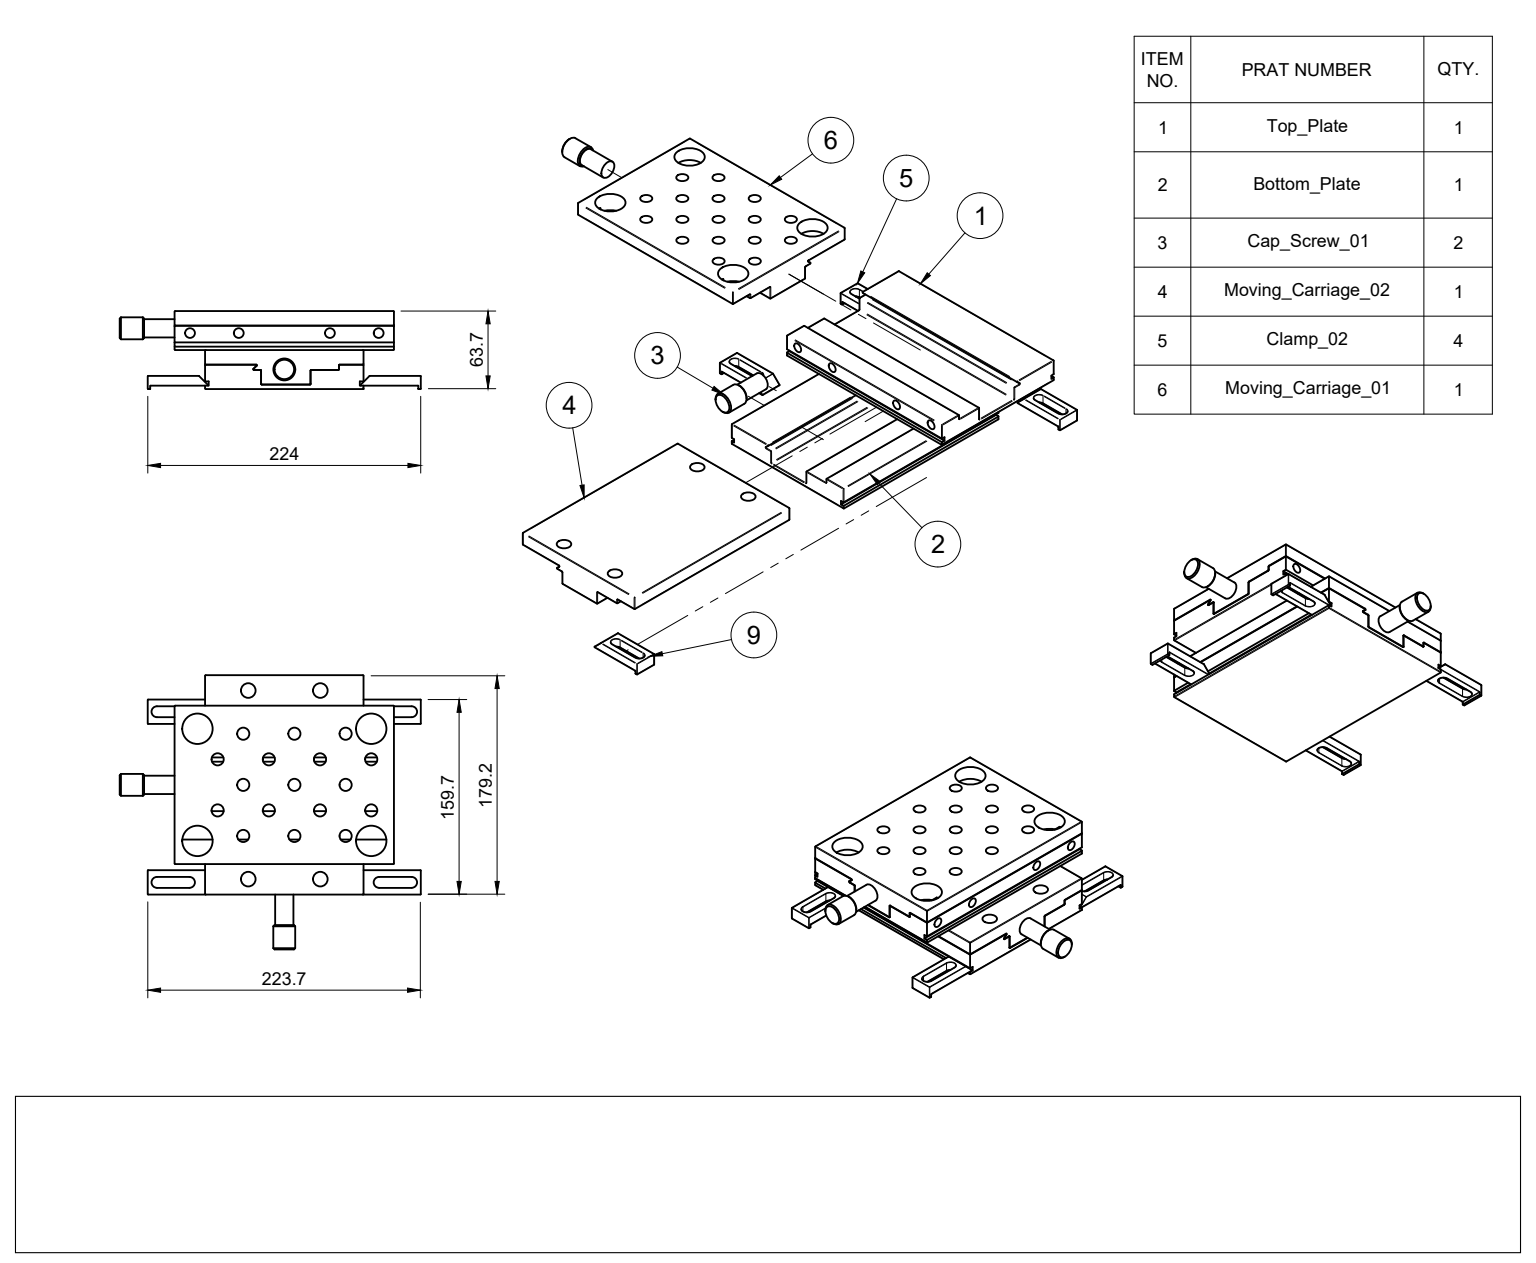
ISO-10303-21;
HEADER;
/* Generated by software containing ST-Developer
 * from STEP Tools, Inc. (www.steptools.com) 
 */

FILE_DESCRIPTION(
/* description */ (''),
/* implementation_level */ '2;1');

FILE_NAME(
/* name */ 'MAS-274',
/* time_stamp */ '2026-10-22T13:39:42+06:00',
/* author */ (''),
/* organization */ (''),
/* preprocessor_version */ 'ST-DEVELOPER v20.2',
/* originating_system */ 'Autodesk Translation Framework v15.15.0.0',
/* authorisation */ '');

FILE_SCHEMA (('AUTOMOTIVE_DESIGN { 1 0 10303 214 3 1 1 }'));
ENDSEC;

DATA;
#10=MECHANICAL_DESIGN_GEOMETRIC_PRESENTATION_REPRESENTATION('',(#307,#308,
#309,#310,#311,#312,#313,#314,#315,#316),#17836);
#11=ITEM_DEFINED_TRANSFORMATION($,$,#9750,#11022);
#12=ITEM_DEFINED_TRANSFORMATION($,$,#9764,#11023);
#13=ITEM_DEFINED_TRANSFORMATION($,$,#9932,#11024);
#14=ITEM_DEFINED_TRANSFORMATION($,$,#10101,#11025);
#15=ITEM_DEFINED_TRANSFORMATION($,$,#10301,#11026);
#16=ITEM_DEFINED_TRANSFORMATION($,$,#10399,#11027);
#17=ITEM_DEFINED_TRANSFORMATION($,$,#10714,#11028);
#18=ITEM_DEFINED_TRANSFORMATION($,$,#10812,#11029);
#19=ITEM_DEFINED_TRANSFORMATION($,$,#10826,#11030);
#20=ITEM_DEFINED_TRANSFORMATION($,$,#10924,#11031);
#21=(
REPRESENTATION_RELATIONSHIP($,$,#17874,#17873)
REPRESENTATION_RELATIONSHIP_WITH_TRANSFORMATION(#11)
SHAPE_REPRESENTATION_RELATIONSHIP()
);
#22=(
REPRESENTATION_RELATIONSHIP($,$,#17875,#17873)
REPRESENTATION_RELATIONSHIP_WITH_TRANSFORMATION(#12)
SHAPE_REPRESENTATION_RELATIONSHIP()
);
#23=(
REPRESENTATION_RELATIONSHIP($,$,#17876,#17873)
REPRESENTATION_RELATIONSHIP_WITH_TRANSFORMATION(#13)
SHAPE_REPRESENTATION_RELATIONSHIP()
);
#24=(
REPRESENTATION_RELATIONSHIP($,$,#17877,#17873)
REPRESENTATION_RELATIONSHIP_WITH_TRANSFORMATION(#14)
SHAPE_REPRESENTATION_RELATIONSHIP()
);
#25=(
REPRESENTATION_RELATIONSHIP($,$,#17878,#17873)
REPRESENTATION_RELATIONSHIP_WITH_TRANSFORMATION(#15)
SHAPE_REPRESENTATION_RELATIONSHIP()
);
#26=(
REPRESENTATION_RELATIONSHIP($,$,#17879,#17873)
REPRESENTATION_RELATIONSHIP_WITH_TRANSFORMATION(#16)
SHAPE_REPRESENTATION_RELATIONSHIP()
);
#27=(
REPRESENTATION_RELATIONSHIP($,$,#17880,#17873)
REPRESENTATION_RELATIONSHIP_WITH_TRANSFORMATION(#17)
SHAPE_REPRESENTATION_RELATIONSHIP()
);
#28=(
REPRESENTATION_RELATIONSHIP($,$,#17881,#17873)
REPRESENTATION_RELATIONSHIP_WITH_TRANSFORMATION(#18)
SHAPE_REPRESENTATION_RELATIONSHIP()
);
#29=(
REPRESENTATION_RELATIONSHIP($,$,#17882,#17873)
REPRESENTATION_RELATIONSHIP_WITH_TRANSFORMATION(#19)
SHAPE_REPRESENTATION_RELATIONSHIP()
);
#30=(
REPRESENTATION_RELATIONSHIP($,$,#17883,#17873)
REPRESENTATION_RELATIONSHIP_WITH_TRANSFORMATION(#20)
SHAPE_REPRESENTATION_RELATIONSHIP()
);
#31=CONTEXT_DEPENDENT_SHAPE_REPRESENTATION(#21,#17863);
#32=CONTEXT_DEPENDENT_SHAPE_REPRESENTATION(#22,#17864);
#33=CONTEXT_DEPENDENT_SHAPE_REPRESENTATION(#23,#17865);
#34=CONTEXT_DEPENDENT_SHAPE_REPRESENTATION(#24,#17866);
#35=CONTEXT_DEPENDENT_SHAPE_REPRESENTATION(#25,#17867);
#36=CONTEXT_DEPENDENT_SHAPE_REPRESENTATION(#26,#17868);
#37=CONTEXT_DEPENDENT_SHAPE_REPRESENTATION(#27,#17869);
#38=CONTEXT_DEPENDENT_SHAPE_REPRESENTATION(#28,#17870);
#39=CONTEXT_DEPENDENT_SHAPE_REPRESENTATION(#29,#17871);
#40=CONTEXT_DEPENDENT_SHAPE_REPRESENTATION(#30,#17872);
#41=NEXT_ASSEMBLY_USAGE_OCCURRENCE('Cap_Screw_01:1','Cap_Screw_01:1',
'Cap_Screw_01:1',#17885,#17886,'Cap_Screw_01:1');
#42=NEXT_ASSEMBLY_USAGE_OCCURRENCE('Bottom_Plate:1','Bottom_Plate:1',
'Bottom_Plate:1',#17885,#17887,'Bottom_Plate:1');
#43=NEXT_ASSEMBLY_USAGE_OCCURRENCE('Moving_Carriage_02:1',
'Moving_Carriage_02:1','Moving_Carriage_02:1',#17885,#17888,
'Moving_Carriage_02:1');
#44=NEXT_ASSEMBLY_USAGE_OCCURRENCE('Top_Plate:1','Top_Plate:1',
'Top_Plate:1',#17885,#17889,'Top_Plate:1');
#45=NEXT_ASSEMBLY_USAGE_OCCURRENCE('Clamp_02:1','Clamp_02:1',
'Clamp_02:1',#17885,#17890,'Clamp_02:1');
#46=NEXT_ASSEMBLY_USAGE_OCCURRENCE('Moving_Carriage_01:1',
'Moving_Carriage_01:1','Moving_Carriage_01:1',#17885,#17891,
'Moving_Carriage_01:1');
#47=NEXT_ASSEMBLY_USAGE_OCCURRENCE('Clamp_01:1','Clamp_01:1',
'Clamp_01:1',#17885,#17892,'Clamp_01:1');
#48=NEXT_ASSEMBLY_USAGE_OCCURRENCE('Cap_Screw_02:1','Cap_Screw_02:1',
'Cap_Screw_02:1',#17885,#17893,'Cap_Screw_02:1');
#49=NEXT_ASSEMBLY_USAGE_OCCURRENCE('Clamp_03:1','Clamp_03:1',
'Clamp_03:1',#17885,#17894,'Clamp_03:1');
#50=NEXT_ASSEMBLY_USAGE_OCCURRENCE('Clamp_04:1','Clamp_04:1',
'Clamp_04:1',#17885,#17895,'Clamp_04:1');
#51=B_SPLINE_CURVE_WITH_KNOTS('',3,(#15627,#15628,#15629,#15630,#15631,
#15632,#15633,#15634,#15635,#15636),.UNSPECIFIED.,.F.,.F.,(4,2,2,2,4),(0.150795783066297,
0.169644465291242,0.188493147516186,0.207360358779659,0.226227570043131),
 .UNSPECIFIED.);
#52=B_SPLINE_CURVE_WITH_KNOTS('',3,(#15640,#15641,#15642,#15643,#15644,
#15645,#15646,#15647,#15648,#15649),.UNSPECIFIED.,.F.,.F.,(4,2,2,2,4),(0.0757694987047649,
0.0947120945274103,0.113654690350056,0.1325089994291,0.151363308508144),
 .UNSPECIFIED.);
#53=B_SPLINE_CURVE_WITH_KNOTS('',3,(#15653,#15654,#15655,#15656,#15657,
#15658,#15659,#15660,#15661,#15662),.UNSPECIFIED.,.F.,.F.,(4,2,2,2,4),(0.151363299946195,
0.170217609025239,0.189071918104283,0.208014513926928,0.226957109749574),
 .UNSPECIFIED.);
#54=B_SPLINE_CURVE_WITH_KNOTS('',3,(#15666,#15667,#15668,#15669,#15670,
#15671,#15672,#15673,#15674,#15675),.UNSPECIFIED.,.F.,.F.,(4,2,2,2,4),(0.0753639993742339,
0.0942312106377064,0.113098421901179,0.131947104126123,0.150795786351068),
 .UNSPECIFIED.);
#55=B_SPLINE_CURVE_WITH_KNOTS('',3,(#15742,#15743,#15744,#15745,#15746,
#15747,#15748,#15749,#15750,#15751),.UNSPECIFIED.,.F.,.F.,(4,2,2,2,4),(0.161501820430177,
0.181202019666624,0.200902218903071,0.22218706551677,0.243471912130469),
 .UNSPECIFIED.);
#56=B_SPLINE_CURVE_WITH_KNOTS('',3,(#15755,#15756,#15757,#15758,#15759,
#15760,#15761,#15762,#15763,#15764),.UNSPECIFIED.,.F.,.F.,(4,2,2,2,4),(0.0930675005857176,
0.116580531967157,0.140093563348597,0.159964165564683,0.179834767780769),
 .UNSPECIFIED.);
#57=B_SPLINE_CURVE_WITH_KNOTS('',3,(#15768,#15769,#15770,#15771,#15772,
#15773,#15774,#15775,#15776,#15777),.UNSPECIFIED.,.F.,.F.,(4,2,2,2,4),(0.179821549944371,
0.199692152160457,0.219562754376543,0.243075785757983,0.266588817139422),
 .UNSPECIFIED.);
#58=B_SPLINE_CURVE_WITH_KNOTS('',3,(#15780,#15781,#15782,#15783,#15784,
#15785,#15786,#15787,#15788,#15789),.UNSPECIFIED.,.F.,.F.,(4,2,2,2,4),(0.0795500677920486,
0.100834914405747,0.122119761019446,0.141819960255893,0.16152015949234),
 .UNSPECIFIED.);
#59=B_SPLINE_CURVE_WITH_KNOTS('',3,(#15810,#15811,#15812,#15813,#15814,
#15815,#15816,#15817,#15818,#15819),.UNSPECIFIED.,.F.,.F.,(4,2,2,2,4),(0.150807296394123,
0.169656833408643,0.188506370423163,0.207379164314979,0.226251958206795),
 .UNSPECIFIED.);
#60=B_SPLINE_CURVE_WITH_KNOTS('',3,(#15822,#15823,#15824,#15825,#15826,
#15827,#15828,#15829,#15830,#15831),.UNSPECIFIED.,.F.,.F.,(4,2,2,2,4),(-0.0760046501525728,
-0.0568078920652052,-0.0376111339778377,-0.0188055669889188,0.),
 .UNSPECIFIED.);
#61=B_SPLINE_CURVE_WITH_KNOTS('',3,(#15833,#15834,#15835,#15836,#15837,
#15838,#15839,#15840,#15841,#15842),.UNSPECIFIED.,.F.,.F.,(4,2,2,2,4),(0.,
0.0188055669889188,0.0376111339778377,0.0568078920652052,0.0760046501525728),
 .UNSPECIFIED.);
#62=B_SPLINE_CURVE_WITH_KNOTS('',3,(#15846,#15847,#15848,#15849,#15850,
#15851,#15852,#15853,#15854,#15855),.UNSPECIFIED.,.F.,.F.,(4,2,2,2,4),(0.0753626345814508,
0.0942354284732671,0.113108222365083,0.131957759379603,0.150807296394123),
 .UNSPECIFIED.);
#63=B_SPLINE_CURVE_WITH_KNOTS('',3,(#15871,#15872,#15873,#15874,#15875,
#15876,#15877,#15878,#15879,#15880),.UNSPECIFIED.,.F.,.F.,(4,2,2,2,4),(0.150807296394123,
0.169656833408643,0.188506370423163,0.207379164314979,0.226251958206795),
 .UNSPECIFIED.);
#64=B_SPLINE_CURVE_WITH_KNOTS('',3,(#15883,#15884,#15885,#15886,#15887,
#15888,#15889,#15890,#15891,#15892),.UNSPECIFIED.,.F.,.F.,(4,2,2,2,4),(-0.0760046501525727,
-0.0568078920652052,-0.0376111339778377,-0.0188055669889188,0.),
 .UNSPECIFIED.);
#65=B_SPLINE_CURVE_WITH_KNOTS('',3,(#15894,#15895,#15896,#15897,#15898,
#15899,#15900,#15901,#15902,#15903),.UNSPECIFIED.,.F.,.F.,(4,2,2,2,4),(0.,
0.0188055669889188,0.0376111339778377,0.0568078920652052,0.0760046501525728),
 .UNSPECIFIED.);
#66=B_SPLINE_CURVE_WITH_KNOTS('',3,(#15907,#15908,#15909,#15910,#15911,
#15912,#15913,#15914,#15915,#15916),.UNSPECIFIED.,.F.,.F.,(4,2,2,2,4),(0.0753626345814508,
0.0942354284732671,0.113108222365083,0.131957759379603,0.150807296394123),
 .UNSPECIFIED.);
#67=B_SPLINE_CURVE_WITH_KNOTS('',3,(#15932,#15933,#15934,#15935,#15936,
#15937,#15938,#15939,#15940,#15941),.UNSPECIFIED.,.F.,.F.,(4,2,2,2,4),(0.150807296394123,
0.169656833408643,0.188506370423163,0.207379164314979,0.226251958206795),
 .UNSPECIFIED.);
#68=B_SPLINE_CURVE_WITH_KNOTS('',3,(#15944,#15945,#15946,#15947,#15948,
#15949,#15950,#15951,#15952,#15953),.UNSPECIFIED.,.F.,.F.,(4,2,2,2,4),(-0.0760046501525728,
-0.0568078920652053,-0.0376111339778377,-0.0188055669889188,0.),
 .UNSPECIFIED.);
#69=B_SPLINE_CURVE_WITH_KNOTS('',3,(#15955,#15956,#15957,#15958,#15959,
#15960,#15961,#15962,#15963,#15964),.UNSPECIFIED.,.F.,.F.,(4,2,2,2,4),(0.,
0.0188055669889189,0.0376111339778377,0.0568078920652053,0.0760046501525728),
 .UNSPECIFIED.);
#70=B_SPLINE_CURVE_WITH_KNOTS('',3,(#15968,#15969,#15970,#15971,#15972,
#15973,#15974,#15975,#15976,#15977),.UNSPECIFIED.,.F.,.F.,(4,2,2,2,4),(0.0753626345814508,
0.0942354284732671,0.113108222365083,0.131957759379603,0.150807296394123),
 .UNSPECIFIED.);
#71=B_SPLINE_CURVE_WITH_KNOTS('',3,(#15990,#15991,#15992,#15993,#15994,
#15995,#15996,#15997,#15998,#15999),.UNSPECIFIED.,.F.,.F.,(4,2,2,2,4),(0.161501820430177,
0.181202019666624,0.200902218903071,0.22218706551677,0.243471912130469),
 .UNSPECIFIED.);
#72=B_SPLINE_CURVE_WITH_KNOTS('',3,(#16003,#16004,#16005,#16006,#16007,
#16008,#16009,#16010,#16011,#16012),.UNSPECIFIED.,.F.,.F.,(4,2,2,2,4),(0.0930675005857173,
0.116580531967157,0.140093563348596,0.159964165564682,0.179834767780769),
 .UNSPECIFIED.);
#73=B_SPLINE_CURVE_WITH_KNOTS('',3,(#16016,#16017,#16018,#16019,#16020,
#16021,#16022,#16023,#16024,#16025),.UNSPECIFIED.,.F.,.F.,(4,2,2,2,4),(0.17982154994437,
0.199692152160456,0.219562754376542,0.243075785757982,0.266588817139421),
 .UNSPECIFIED.);
#74=B_SPLINE_CURVE_WITH_KNOTS('',3,(#16028,#16029,#16030,#16031,#16032,
#16033,#16034,#16035,#16036,#16037),.UNSPECIFIED.,.F.,.F.,(4,2,2,2,4),(0.0795500677920484,
0.100834914405747,0.122119761019446,0.141819960255893,0.16152015949234),
 .UNSPECIFIED.);
#75=B_SPLINE_CURVE_WITH_KNOTS('',3,(#16052,#16053,#16054,#16055,#16056,
#16057,#16058,#16059,#16060,#16061),.UNSPECIFIED.,.F.,.F.,(4,2,2,2,4),(0.150807296394123,
0.169656833408643,0.188506370423163,0.207379164314979,0.226251958206795),
 .UNSPECIFIED.);
#76=B_SPLINE_CURVE_WITH_KNOTS('',3,(#16064,#16065,#16066,#16067,#16068,
#16069,#16070,#16071,#16072,#16073),.UNSPECIFIED.,.F.,.F.,(4,2,2,2,4),(-0.0760046501525727,
-0.0568078920652052,-0.0376111339778377,-0.0188055669889188,0.),
 .UNSPECIFIED.);
#77=B_SPLINE_CURVE_WITH_KNOTS('',3,(#16075,#16076,#16077,#16078,#16079,
#16080,#16081,#16082,#16083,#16084),.UNSPECIFIED.,.F.,.F.,(4,2,2,2,4),(0.,
0.0188055669889188,0.0376111339778377,0.0568078920652052,0.0760046501525727),
 .UNSPECIFIED.);
#78=B_SPLINE_CURVE_WITH_KNOTS('',3,(#16088,#16089,#16090,#16091,#16092,
#16093,#16094,#16095,#16096,#16097),.UNSPECIFIED.,.F.,.F.,(4,2,2,2,4),(0.0753626345814508,
0.0942354284732671,0.113108222365083,0.131957759379603,0.150807296394123),
 .UNSPECIFIED.);
#79=B_SPLINE_CURVE_WITH_KNOTS('',3,(#16107,#16108,#16109,#16110,#16111,
#16112,#16113,#16114,#16115,#16116),.UNSPECIFIED.,.F.,.F.,(4,2,2,2,4),(0.154001562562628,
0.172841700119288,0.191681837675949,0.211603838452167,0.231525839228385),
 .UNSPECIFIED.);
#80=B_SPLINE_CURVE_WITH_KNOTS('',3,(#16120,#16121,#16122,#16123,#16124,
#16125,#16126,#16127,#16128,#16129),.UNSPECIFIED.,.F.,.F.,(4,2,2,2,4),(-0.0796560912226912,
-0.0585074655832388,-0.0373588399437865,-0.0186794199718932,0.),
 .UNSPECIFIED.);
#81=B_SPLINE_CURVE_WITH_KNOTS('',3,(#16133,#16134,#16135,#16136,#16137,
#16138,#16139,#16140,#16141,#16142),.UNSPECIFIED.,.F.,.F.,(4,2,2,2,4),(0.,
0.0186794199718932,0.0373588399437865,0.0585074655832388,0.0796560912226912),
 .UNSPECIFIED.);
#82=B_SPLINE_CURVE_WITH_KNOTS('',3,(#16146,#16147,#16148,#16149,#16150,
#16151,#16152,#16153,#16154,#16155),.UNSPECIFIED.,.F.,.F.,(4,2,2,2,4),(0.0764772858968706,
0.0963992866730888,0.116321287449307,0.135161425005967,0.154001562562628),
 .UNSPECIFIED.);
#83=B_SPLINE_CURVE_WITH_KNOTS('',3,(#16159,#16160,#16161,#16162,#16163,
#16164,#16165,#16166,#16167,#16168,#16169,#16170,#16171,#16172,#16173,#16174,
#16175,#16176,#16177,#16178,#16179),.UNSPECIFIED.,.F.,.F.,(4,2,2,2,3,2,
2,2,2,4),(-0.0487654213288014,-0.0396424658283718,-0.0198212329141859,-0.00991061645709296,
0.,0.00991061645709312,0.0198212329141862,0.0396424658283725,0.0754755088146795,
0.111308551800987),.UNSPECIFIED.);
#84=B_SPLINE_CURVE_WITH_KNOTS('',3,(#16183,#16184,#16185,#16186,#16187,
#16188,#16189,#16190,#16191,#16192,#16193,#16194,#16195,#16196,#16197,#16198),
 .UNSPECIFIED.,.F.,.F.,(4,2,2,2,2,2,2,4),(0.080261889411958,0.100728357288421,
0.121194825164885,0.139914688841483,0.158634552518082,0.177354416194681,
0.19607427987128,0.196799093526934),.UNSPECIFIED.);
#85=B_SPLINE_CURVE_WITH_KNOTS('',3,(#16202,#16203,#16204,#16205,#16206,
#16207,#16208,#16209,#16210,#16211,#16212,#16213,#16214,#16215,#16216,#16217),
 .UNSPECIFIED.,.F.,.F.,(4,2,2,2,2,2,2,4),(0.120470011509229,0.121194825164884,
0.139914688841482,0.158634552518081,0.17735441619468,0.196074279871279,
0.216540747747742,0.237007215624205),.UNSPECIFIED.);
#86=B_SPLINE_CURVE_WITH_KNOTS('',3,(#16221,#16222,#16223,#16224,#16225,
#16226,#16227,#16228,#16229,#16230,#16231,#16232,#16233,#16234,#16235,#16236,
#16237,#16238,#16239,#16240,#16241),.UNSPECIFIED.,.F.,.F.,(4,2,2,2,2,3,
2,2,2,4),(-0.111308551800987,-0.0754755088146795,-0.0396424658283724,-0.0198212329141862,
-0.00991061645709312,0.,0.00991061645709295,0.0198212329141859,0.0396424658283718,
0.0487654212438806),.UNSPECIFIED.);
#87=B_SPLINE_CURVE_WITH_KNOTS('',3,(#16251,#16252,#16253,#16254,#16255,
#16256,#16257,#16258,#16259,#16260),.UNSPECIFIED.,.F.,.F.,(4,2,2,2,4),(0.150795783066297,
0.169644465291242,0.188493147516186,0.207360358779658,0.226227570043131),
 .UNSPECIFIED.);
#88=B_SPLINE_CURVE_WITH_KNOTS('',3,(#16263,#16264,#16265,#16266,#16267,
#16268,#16269,#16270,#16271,#16272),.UNSPECIFIED.,.F.,.F.,(4,2,2,2,4),(0.0757694987047649,
0.0947120945274103,0.113654690350056,0.1325089994291,0.151363308508144),
 .UNSPECIFIED.);
#89=B_SPLINE_CURVE_WITH_KNOTS('',3,(#16274,#16275,#16276,#16277,#16278,
#16279,#16280,#16281,#16282,#16283),.UNSPECIFIED.,.F.,.F.,(4,2,2,2,4),(0.151363299946195,
0.170217609025239,0.189071918104283,0.208014513926928,0.226957109749573),
 .UNSPECIFIED.);
#90=B_SPLINE_CURVE_WITH_KNOTS('',3,(#16287,#16288,#16289,#16290,#16291,
#16292,#16293,#16294,#16295,#16296),.UNSPECIFIED.,.F.,.F.,(4,2,2,2,4),(0.075363999374234,
0.0942312106377065,0.113098421901179,0.131947104126123,0.150795786351068),
 .UNSPECIFIED.);
#91=B_SPLINE_CURVE_WITH_KNOTS('',3,(#16306,#16307,#16308,#16309,#16310,
#16311,#16312,#16313,#16314,#16315),.UNSPECIFIED.,.F.,.F.,(4,2,2,2,4),(0.154001562562628,
0.172841700119289,0.191681837675949,0.211603838452167,0.231525839228385),
 .UNSPECIFIED.);
#92=B_SPLINE_CURVE_WITH_KNOTS('',3,(#16319,#16320,#16321,#16322,#16323,
#16324,#16325,#16326,#16327,#16328),.UNSPECIFIED.,.F.,.F.,(4,2,2,2,4),(-0.0796560912226911,
-0.0585074655832388,-0.0373588399437865,-0.0186794199718933,0.),
 .UNSPECIFIED.);
#93=B_SPLINE_CURVE_WITH_KNOTS('',3,(#16332,#16333,#16334,#16335,#16336,
#16337,#16338,#16339,#16340,#16341),.UNSPECIFIED.,.F.,.F.,(4,2,2,2,4),(0.,
0.0186794199718933,0.0373588399437865,0.0585074655832388,0.0796560912226911),
 .UNSPECIFIED.);
#94=B_SPLINE_CURVE_WITH_KNOTS('',3,(#16345,#16346,#16347,#16348,#16349,
#16350,#16351,#16352,#16353,#16354),.UNSPECIFIED.,.F.,.F.,(4,2,2,2,4),(0.0764772858968706,
0.0963992866730888,0.116321287449307,0.135161425005967,0.154001562562628),
 .UNSPECIFIED.);
#95=B_SPLINE_CURVE_WITH_KNOTS('',3,(#16358,#16359,#16360,#16361,#16362,
#16363,#16364,#16365,#16366,#16367,#16368,#16369,#16370,#16371,#16372,#16373,
#16374,#16375,#16376,#16377,#16378),.UNSPECIFIED.,.F.,.F.,(4,2,2,2,3,2,
2,2,2,4),(-0.0487654213288006,-0.0396424658283715,-0.0198212329141857,-0.00991061645709285,
0.,0.00991061645709304,0.0198212329141861,0.0396424658283721,0.0754755088146788,
0.111308551800986),.UNSPECIFIED.);
#96=B_SPLINE_CURVE_WITH_KNOTS('',3,(#16382,#16383,#16384,#16385,#16386,
#16387,#16388,#16389,#16390,#16391,#16392,#16393,#16394,#16395,#16396,#16397),
 .UNSPECIFIED.,.F.,.F.,(4,2,2,2,2,2,2,4),(0.080261889411958,0.100728357288421,
0.121194825164885,0.139914688841484,0.158634552518082,0.177354416194681,
0.19607427987128,0.196799093526934),.UNSPECIFIED.);
#97=B_SPLINE_CURVE_WITH_KNOTS('',3,(#16401,#16402,#16403,#16404,#16405,
#16406,#16407,#16408,#16409,#16410,#16411,#16412,#16413,#16414,#16415,#16416),
 .UNSPECIFIED.,.F.,.F.,(4,2,2,2,2,2,2,4),(0.120470011509229,0.121194825164884,
0.139914688841482,0.158634552518081,0.17735441619468,0.196074279871279,
0.216540747747742,0.237007215624205),.UNSPECIFIED.);
#98=B_SPLINE_CURVE_WITH_KNOTS('',3,(#16420,#16421,#16422,#16423,#16424,
#16425,#16426,#16427,#16428,#16429,#16430,#16431,#16432,#16433,#16434,#16435,
#16436,#16437,#16438,#16439,#16440),.UNSPECIFIED.,.F.,.F.,(4,2,2,2,2,3,
2,2,2,4),(-0.111308551800986,-0.0754755088146788,-0.0396424658283722,-0.0198212329141861,
-0.00991061645709307,0.,0.00991061645709287,0.0198212329141857,0.0396424658283715,
0.0487654212438799),.UNSPECIFIED.);
#99=B_SPLINE_CURVE_WITH_KNOTS('',3,(#16450,#16451,#16452,#16453,#16454,
#16455,#16456,#16457,#16458,#16459),.UNSPECIFIED.,.F.,.F.,(4,2,2,2,4),(0.154001562562628,
0.172841700119288,0.191681837675949,0.211603838452167,0.231525839228385),
 .UNSPECIFIED.);
#100=B_SPLINE_CURVE_WITH_KNOTS('',3,(#16463,#16464,#16465,#16466,#16467,
#16468,#16469,#16470,#16471,#16472),.UNSPECIFIED.,.F.,.F.,(4,2,2,2,4),(-0.0796560912226909,
-0.0585074655832387,-0.0373588399437865,-0.0186794199718933,0.),
 .UNSPECIFIED.);
#101=B_SPLINE_CURVE_WITH_KNOTS('',3,(#16476,#16477,#16478,#16479,#16480,
#16481,#16482,#16483,#16484,#16485),.UNSPECIFIED.,.F.,.F.,(4,2,2,2,4),(0.,
0.0186794199718933,0.0373588399437866,0.0585074655832387,0.0796560912226909),
 .UNSPECIFIED.);
#102=B_SPLINE_CURVE_WITH_KNOTS('',3,(#16489,#16490,#16491,#16492,#16493,
#16494,#16495,#16496,#16497,#16498),.UNSPECIFIED.,.F.,.F.,(4,2,2,2,4),(0.0764772858968707,
0.0963992866730888,0.116321287449307,0.135161425005967,0.154001562562628),
 .UNSPECIFIED.);
#103=B_SPLINE_CURVE_WITH_KNOTS('',3,(#16502,#16503,#16504,#16505,#16506,
#16507,#16508,#16509,#16510,#16511,#16512,#16513,#16514,#16515,#16516,#16517,
#16518,#16519,#16520,#16521,#16522),.UNSPECIFIED.,.F.,.F.,(4,2,2,2,3,2,
2,2,2,4),(-0.0487654213288013,-0.0396424658283719,-0.019821232914186,-0.00991061645709301,
0.,0.00991061645709316,0.0198212329141863,0.0396424658283726,0.0754755088146797,
0.111308551800987),.UNSPECIFIED.);
#104=B_SPLINE_CURVE_WITH_KNOTS('',3,(#16526,#16527,#16528,#16529,#16530,
#16531,#16532,#16533,#16534,#16535,#16536,#16537,#16538,#16539,#16540,#16541),
 .UNSPECIFIED.,.F.,.F.,(4,2,2,2,2,2,2,4),(0.080261889411958,0.100728357288421,
0.121194825164885,0.139914688841484,0.158634552518082,0.177354416194681,
0.19607427987128,0.196799093526934),.UNSPECIFIED.);
#105=B_SPLINE_CURVE_WITH_KNOTS('',3,(#16545,#16546,#16547,#16548,#16549,
#16550,#16551,#16552,#16553,#16554,#16555,#16556,#16557,#16558,#16559,#16560),
 .UNSPECIFIED.,.F.,.F.,(4,2,2,2,2,2,2,4),(0.120470011509229,0.121194825164884,
0.139914688841482,0.158634552518081,0.17735441619468,0.196074279871279,
0.216540747747742,0.237007215624205),.UNSPECIFIED.);
#106=B_SPLINE_CURVE_WITH_KNOTS('',3,(#16564,#16565,#16566,#16567,#16568,
#16569,#16570,#16571,#16572,#16573,#16574,#16575,#16576,#16577,#16578,#16579,
#16580,#16581,#16582,#16583,#16584),.UNSPECIFIED.,.F.,.F.,(4,2,2,2,2,3,
2,2,2,4),(-0.111308551800987,-0.0754755088146797,-0.0396424658283726,-0.0198212329141863,
-0.00991061645709312,0.,0.00991061645709299,0.019821232914186,0.039642465828372,
0.0487654212438805),.UNSPECIFIED.);
#107=B_SPLINE_CURVE_WITH_KNOTS('',3,(#16594,#16595,#16596,#16597,#16598,
#16599,#16600,#16601,#16602,#16603),.UNSPECIFIED.,.F.,.F.,(4,2,2,2,4),(0.154001562562628,
0.172841700119288,0.191681837675949,0.211603838452167,0.231525839228385),
 .UNSPECIFIED.);
#108=B_SPLINE_CURVE_WITH_KNOTS('',3,(#16607,#16608,#16609,#16610,#16611,
#16612,#16613,#16614,#16615,#16616),.UNSPECIFIED.,.F.,.F.,(4,2,2,2,4),(-0.0796560912226908,
-0.0585074655832387,-0.0373588399437865,-0.0186794199718933,0.),
 .UNSPECIFIED.);
#109=B_SPLINE_CURVE_WITH_KNOTS('',3,(#16620,#16621,#16622,#16623,#16624,
#16625,#16626,#16627,#16628,#16629),.UNSPECIFIED.,.F.,.F.,(4,2,2,2,4),(0.,
0.0186794199718932,0.0373588399437865,0.0585074655832387,0.0796560912226908),
 .UNSPECIFIED.);
#110=B_SPLINE_CURVE_WITH_KNOTS('',3,(#16633,#16634,#16635,#16636,#16637,
#16638,#16639,#16640,#16641,#16642),.UNSPECIFIED.,.F.,.F.,(4,2,2,2,4),(0.0764772858968705,
0.0963992866730887,0.116321287449307,0.135161425005967,0.154001562562628),
 .UNSPECIFIED.);
#111=B_SPLINE_CURVE_WITH_KNOTS('',3,(#16646,#16647,#16648,#16649,#16650,
#16651,#16652,#16653,#16654,#16655,#16656,#16657,#16658,#16659,#16660,#16661,
#16662,#16663,#16664,#16665,#16666),.UNSPECIFIED.,.F.,.F.,(4,2,2,2,3,2,
2,2,2,4),(-0.0487654213288016,-0.0396424658283713,-0.0198212329141857,-0.00991061645709285,
0.,0.0099106164570932,0.0198212329141864,0.0396424658283728,0.0754755088146802,
0.111308551800988),.UNSPECIFIED.);
#112=B_SPLINE_CURVE_WITH_KNOTS('',3,(#16670,#16671,#16672,#16673,#16674,
#16675,#16676,#16677,#16678,#16679,#16680,#16681,#16682,#16683,#16684,#16685),
 .UNSPECIFIED.,.F.,.F.,(4,2,2,2,2,2,2,4),(0.0802618894119582,0.100728357288421,
0.121194825164885,0.139914688841483,0.158634552518082,0.177354416194681,
0.19607427987128,0.196799093526934),.UNSPECIFIED.);
#113=B_SPLINE_CURVE_WITH_KNOTS('',3,(#16689,#16690,#16691,#16692,#16693,
#16694,#16695,#16696,#16697,#16698,#16699,#16700,#16701,#16702,#16703,#16704),
 .UNSPECIFIED.,.F.,.F.,(4,2,2,2,2,2,2,4),(0.12047001150923,0.121194825164884,
0.139914688841483,0.158634552518082,0.17735441619468,0.196074279871279,
0.216540747747742,0.237007215624206),.UNSPECIFIED.);
#114=B_SPLINE_CURVE_WITH_KNOTS('',3,(#16708,#16709,#16710,#16711,#16712,
#16713,#16714,#16715,#16716,#16717,#16718,#16719,#16720,#16721,#16722,#16723,
#16724,#16725,#16726,#16727,#16728),.UNSPECIFIED.,.F.,.F.,(4,2,2,2,2,3,
2,2,2,4),(-0.111308551800987,-0.0754755088146801,-0.0396424658283728,-0.0198212329141864,
-0.00991061645709318,0.,0.00991061645709283,0.0198212329141857,0.0396424658283713,
0.0487654212438809),.UNSPECIFIED.);
#115=B_SPLINE_CURVE_WITH_KNOTS('',3,(#16741,#16742,#16743,#16744,#16745,
#16746,#16747,#16748,#16749,#16750),.UNSPECIFIED.,.F.,.F.,(4,2,2,2,4),(0.161501820430177,
0.181202019666624,0.200902218903071,0.22218706551677,0.243471912130469),
 .UNSPECIFIED.);
#116=B_SPLINE_CURVE_WITH_KNOTS('',3,(#16754,#16755,#16756,#16757,#16758,
#16759,#16760,#16761,#16762,#16763),.UNSPECIFIED.,.F.,.F.,(4,2,2,2,4),(0.0930675005857169,
0.116580531967156,0.140093563348596,0.159964165564682,0.179834767780768),
 .UNSPECIFIED.);
#117=B_SPLINE_CURVE_WITH_KNOTS('',3,(#16767,#16768,#16769,#16770,#16771,
#16772,#16773,#16774,#16775,#16776),.UNSPECIFIED.,.F.,.F.,(4,2,2,2,4),(0.17982154994437,
0.199692152160456,0.219562754376542,0.243075785757982,0.266588817139421),
 .UNSPECIFIED.);
#118=B_SPLINE_CURVE_WITH_KNOTS('',3,(#16779,#16780,#16781,#16782,#16783,
#16784,#16785,#16786,#16787,#16788),.UNSPECIFIED.,.F.,.F.,(4,2,2,2,4),(0.0795500677920484,
0.100834914405747,0.122119761019446,0.141819960255893,0.16152015949234),
 .UNSPECIFIED.);
#119=SPHERICAL_SURFACE('',#9812,0.499999999999998);
#120=SPHERICAL_SURFACE('',#9816,0.499999999999998);
#121=SPHERICAL_SURFACE('',#9821,0.5);
#122=SPHERICAL_SURFACE('',#9827,0.499999999999998);
#123=SPHERICAL_SURFACE('',#9837,0.500000000000007);
#124=SPHERICAL_SURFACE('',#9846,0.500000000000007);
#125=SPHERICAL_SURFACE('',#9859,0.5);
#126=SPHERICAL_SURFACE('',#9863,0.5);
#127=SPHERICAL_SURFACE('',#9868,0.5);
#128=SPHERICAL_SURFACE('',#9874,0.5);
#129=SPHERICAL_SURFACE('',#9883,0.500000000000007);
#130=SPHERICAL_SURFACE('',#9891,0.500000000000007);
#131=SPHERICAL_SURFACE('',#9896,0.500000000000007);
#132=SPHERICAL_SURFACE('',#9902,0.499999999999998);
#133=SPHERICAL_SURFACE('',#9947,0.500000000000025);
#134=SPHERICAL_SURFACE('',#9951,0.500000000000005);
#135=SPHERICAL_SURFACE('',#9977,0.500000000000007);
#136=SPHERICAL_SURFACE('',#9982,0.499999999999998);
#137=SPHERICAL_SURFACE('',#9987,0.500000000000007);
#138=SPHERICAL_SURFACE('',#9991,0.500000000000007);
#139=SPHERICAL_SURFACE('',#9996,0.500000000000007);
#140=SPHERICAL_SURFACE('',#10001,0.500000000000007);
#141=SPHERICAL_SURFACE('',#10006,0.500000000000007);
#142=SPHERICAL_SURFACE('',#10010,0.500000000000007);
#143=SPHERICAL_SURFACE('',#10021,0.500000000000007);
#144=SPHERICAL_SURFACE('',#10030,0.500000000000007);
#145=SPHERICAL_SURFACE('',#10034,0.500000000000007);
#146=SPHERICAL_SURFACE('',#10039,0.499999999999998);
#147=SPHERICAL_SURFACE('',#10043,0.500000000000007);
#148=SPHERICAL_SURFACE('',#10047,0.499999999999998);
#149=SPHERICAL_SURFACE('',#10181,0.499999999999998);
#150=SPHERICAL_SURFACE('',#10185,0.499999999999998);
#151=SPHERICAL_SURFACE('',#10190,0.5);
#152=SPHERICAL_SURFACE('',#10196,0.499999999999998);
#153=SPHERICAL_SURFACE('',#10206,0.500000000000007);
#154=SPHERICAL_SURFACE('',#10215,0.500000000000007);
#155=SPHERICAL_SURFACE('',#10228,0.5);
#156=SPHERICAL_SURFACE('',#10232,0.5);
#157=SPHERICAL_SURFACE('',#10237,0.5);
#158=SPHERICAL_SURFACE('',#10243,0.5);
#159=SPHERICAL_SURFACE('',#10252,0.500000000000007);
#160=SPHERICAL_SURFACE('',#10260,0.500000000000007);
#161=SPHERICAL_SURFACE('',#10265,0.500000000000007);
#162=SPHERICAL_SURFACE('',#10271,0.499999999999998);
#163=SPHERICAL_SURFACE('',#10323,0.299999999999994);
#164=SPHERICAL_SURFACE('',#10334,0.3);
#165=SPHERICAL_SURFACE('',#10338,0.299999999999994);
#166=SPHERICAL_SURFACE('',#10343,0.3);
#167=SPHERICAL_SURFACE('',#10347,0.300000000000011);
#168=SPHERICAL_SURFACE('',#10351,0.300000000000003);
#169=SPHERICAL_SURFACE('',#10355,0.299999999999994);
#170=SPHERICAL_SURFACE('',#10360,0.300000000000011);
#171=SPHERICAL_SURFACE('',#10585,0.500000000000025);
#172=SPHERICAL_SURFACE('',#10588,0.500000000000005);
#173=SPHERICAL_SURFACE('',#10609,0.500000000000007);
#174=SPHERICAL_SURFACE('',#10613,0.499999999999998);
#175=SPHERICAL_SURFACE('',#10618,0.500000000000007);
#176=SPHERICAL_SURFACE('',#10621,0.500000000000007);
#177=SPHERICAL_SURFACE('',#10626,0.500000000000007);
#178=SPHERICAL_SURFACE('',#10630,0.500000000000007);
#179=SPHERICAL_SURFACE('',#10635,0.500000000000007);
#180=SPHERICAL_SURFACE('',#10638,0.500000000000007);
#181=SPHERICAL_SURFACE('',#10648,0.500000000000007);
#182=SPHERICAL_SURFACE('',#10656,0.500000000000007);
#183=SPHERICAL_SURFACE('',#10660,0.500000000000007);
#184=SPHERICAL_SURFACE('',#10664,0.499999999999998);
#185=SPHERICAL_SURFACE('',#10668,0.500000000000007);
#186=SPHERICAL_SURFACE('',#10671,0.499999999999998);
#187=SPHERICAL_SURFACE('',#10736,0.299999999999994);
#188=SPHERICAL_SURFACE('',#10747,0.3);
#189=SPHERICAL_SURFACE('',#10751,0.299999999999994);
#190=SPHERICAL_SURFACE('',#10756,0.3);
#191=SPHERICAL_SURFACE('',#10760,0.300000000000011);
#192=SPHERICAL_SURFACE('',#10764,0.300000000000003);
#193=SPHERICAL_SURFACE('',#10768,0.299999999999994);
#194=SPHERICAL_SURFACE('',#10773,0.300000000000011);
#195=SPHERICAL_SURFACE('',#10848,0.299999999999994);
#196=SPHERICAL_SURFACE('',#10859,0.3);
#197=SPHERICAL_SURFACE('',#10863,0.299999999999994);
#198=SPHERICAL_SURFACE('',#10868,0.3);
#199=SPHERICAL_SURFACE('',#10872,0.300000000000011);
#200=SPHERICAL_SURFACE('',#10876,0.300000000000003);
#201=SPHERICAL_SURFACE('',#10880,0.299999999999994);
#202=SPHERICAL_SURFACE('',#10885,0.300000000000011);
#203=SPHERICAL_SURFACE('',#10946,0.299999999999994);
#204=SPHERICAL_SURFACE('',#10957,0.3);
#205=SPHERICAL_SURFACE('',#10961,0.299999999999994);
#206=SPHERICAL_SURFACE('',#10966,0.3);
#207=SPHERICAL_SURFACE('',#10970,0.300000000000011);
#208=SPHERICAL_SURFACE('',#10974,0.300000000000003);
#209=SPHERICAL_SURFACE('',#10978,0.299999999999994);
#210=SPHERICAL_SURFACE('',#10983,0.300000000000011);
#211=TOROIDAL_SURFACE('',#9804,0.999999999999996,0.500000000000007);
#212=TOROIDAL_SURFACE('',#9808,1.,0.500000000000007);
#213=TOROIDAL_SURFACE('',#9833,0.999999999999996,0.500000000000007);
#214=TOROIDAL_SURFACE('',#9840,1.,0.500000000000007);
#215=TOROIDAL_SURFACE('',#9849,1.,0.500000000000007);
#216=TOROIDAL_SURFACE('',#9853,1.,0.500000000000007);
#217=TOROIDAL_SURFACE('',#9879,0.99999999999999,0.500000000000007);
#218=TOROIDAL_SURFACE('',#9887,0.999999999999994,0.5);
#219=TOROIDAL_SURFACE('',#9955,1.,0.5);
#220=TOROIDAL_SURFACE('',#9961,1.,0.500000000000002);
#221=TOROIDAL_SURFACE('',#9966,0.999999999999996,0.499999999999998);
#222=TOROIDAL_SURFACE('',#9971,1.,0.499999999999998);
#223=TOROIDAL_SURFACE('',#10015,0.999999999999999,0.499999999999998);
#224=TOROIDAL_SURFACE('',#10025,1.,0.499999999999998);
#225=TOROIDAL_SURFACE('',#10051,0.999999999999996,0.499999999999998);
#226=TOROIDAL_SURFACE('',#10058,1.00000000000001,0.500000000000007);
#227=TOROIDAL_SURFACE('',#10173,0.999999999999996,0.500000000000007);
#228=TOROIDAL_SURFACE('',#10177,1.,0.500000000000007);
#229=TOROIDAL_SURFACE('',#10202,0.999999999999996,0.500000000000007);
#230=TOROIDAL_SURFACE('',#10209,1.,0.500000000000007);
#231=TOROIDAL_SURFACE('',#10218,1.,0.500000000000007);
#232=TOROIDAL_SURFACE('',#10222,1.,0.500000000000007);
#233=TOROIDAL_SURFACE('',#10248,0.99999999999999,0.500000000000007);
#234=TOROIDAL_SURFACE('',#10256,0.999999999999994,0.5);
#235=TOROIDAL_SURFACE('',#10305,4.79999999999999,0.3);
#236=TOROIDAL_SURFACE('',#10311,4.79999999999998,0.3);
#237=TOROIDAL_SURFACE('',#10318,0.600000000000001,0.3);
#238=TOROIDAL_SURFACE('',#10327,0.600000000000001,0.300000000000011);
#239=TOROIDAL_SURFACE('',#10390,4.79999999999998,0.3);
#240=TOROIDAL_SURFACE('',#10395,4.79999999999999,0.3);
#241=TOROIDAL_SURFACE('',#10591,1.,0.5);
#242=TOROIDAL_SURFACE('',#10596,1.,0.500000000000002);
#243=TOROIDAL_SURFACE('',#10600,0.999999999999996,0.499999999999998);
#244=TOROIDAL_SURFACE('',#10604,1.,0.499999999999998);
#245=TOROIDAL_SURFACE('',#10643,0.999999999999999,0.499999999999998);
#246=TOROIDAL_SURFACE('',#10652,1.,0.499999999999998);
#247=TOROIDAL_SURFACE('',#10675,0.999999999999996,0.499999999999998);
#248=TOROIDAL_SURFACE('',#10681,1.00000000000001,0.500000000000007);
#249=TOROIDAL_SURFACE('',#10718,4.79999999999999,0.3);
#250=TOROIDAL_SURFACE('',#10724,4.79999999999998,0.3);
#251=TOROIDAL_SURFACE('',#10731,0.600000000000001,0.3);
#252=TOROIDAL_SURFACE('',#10740,0.600000000000001,0.300000000000011);
#253=TOROIDAL_SURFACE('',#10803,4.79999999999998,0.3);
#254=TOROIDAL_SURFACE('',#10808,4.79999999999999,0.3);
#255=TOROIDAL_SURFACE('',#10830,4.79999999999999,0.3);
#256=TOROIDAL_SURFACE('',#10836,4.79999999999998,0.3);
#257=TOROIDAL_SURFACE('',#10843,0.600000000000001,0.3);
#258=TOROIDAL_SURFACE('',#10852,0.600000000000001,0.300000000000011);
#259=TOROIDAL_SURFACE('',#10915,4.79999999999998,0.3);
#260=TOROIDAL_SURFACE('',#10920,4.79999999999999,0.3);
#261=TOROIDAL_SURFACE('',#10928,4.79999999999999,0.3);
#262=TOROIDAL_SURFACE('',#10934,4.79999999999998,0.3);
#263=TOROIDAL_SURFACE('',#10941,0.600000000000001,0.3);
#264=TOROIDAL_SURFACE('',#10950,0.600000000000001,0.300000000000011);
#265=TOROIDAL_SURFACE('',#11013,4.79999999999998,0.3);
#266=TOROIDAL_SURFACE('',#11018,4.79999999999999,0.3);
#267=ELLIPSE('',#9773,0.707106781186543,0.5);
#268=ELLIPSE('',#9779,0.707106781186553,0.5);
#269=ELLIPSE('',#10142,0.707106781186543,0.5);
#270=ELLIPSE('',#10148,0.707106781186553,0.5);
#271=ELLIPSE('',#10333,0.424264068711946,0.3);
#272=ELLIPSE('',#10377,0.424264068711924,0.3);
#273=ELLIPSE('',#10470,7.07106781186548,5.);
#274=ELLIPSE('',#10472,7.07106781186548,5.);
#275=ELLIPSE('',#10483,7.07106781186548,5.);
#276=ELLIPSE('',#10485,7.07106781186548,5.);
#277=ELLIPSE('',#10492,7.07106781186548,5.);
#278=ELLIPSE('',#10494,7.07106781186548,5.);
#279=ELLIPSE('',#10501,7.07106781186548,5.);
#280=ELLIPSE('',#10503,7.07106781186548,5.);
#281=ELLIPSE('',#10746,0.424264068711946,0.3);
#282=ELLIPSE('',#10790,0.424264068711924,0.3);
#283=ELLIPSE('',#10858,0.424264068711946,0.3);
#284=ELLIPSE('',#10902,0.424264068711924,0.3);
#285=ELLIPSE('',#10956,0.424264068711946,0.3);
#286=ELLIPSE('',#11000,0.424264068711924,0.3);
#287=SHAPE_REPRESENTATION_RELATIONSHIP('SRR','None',#17874,#297);
#288=SHAPE_REPRESENTATION_RELATIONSHIP('SRR','None',#17875,#298);
#289=SHAPE_REPRESENTATION_RELATIONSHIP('SRR','None',#17876,#299);
#290=SHAPE_REPRESENTATION_RELATIONSHIP('SRR','None',#17877,#300);
#291=SHAPE_REPRESENTATION_RELATIONSHIP('SRR','None',#17878,#301);
#292=SHAPE_REPRESENTATION_RELATIONSHIP('SRR','None',#17879,#302);
#293=SHAPE_REPRESENTATION_RELATIONSHIP('SRR','None',#17880,#303);
#294=SHAPE_REPRESENTATION_RELATIONSHIP('SRR','None',#17881,#304);
#295=SHAPE_REPRESENTATION_RELATIONSHIP('SRR','None',#17882,#305);
#296=SHAPE_REPRESENTATION_RELATIONSHIP('SRR','None',#17883,#306);
#297=ADVANCED_BREP_SHAPE_REPRESENTATION('',(#317),#17826);
#298=ADVANCED_BREP_SHAPE_REPRESENTATION('',(#318),#17827);
#299=ADVANCED_BREP_SHAPE_REPRESENTATION('',(#319),#17828);
#300=ADVANCED_BREP_SHAPE_REPRESENTATION('',(#320),#17829);
#301=ADVANCED_BREP_SHAPE_REPRESENTATION('',(#321),#17830);
#302=ADVANCED_BREP_SHAPE_REPRESENTATION('',(#322),#17831);
#303=ADVANCED_BREP_SHAPE_REPRESENTATION('',(#323),#17832);
#304=ADVANCED_BREP_SHAPE_REPRESENTATION('',(#324),#17833);
#305=ADVANCED_BREP_SHAPE_REPRESENTATION('',(#325),#17834);
#306=ADVANCED_BREP_SHAPE_REPRESENTATION('',(#326),#17835);
#307=STYLED_ITEM('',(#17980),#317);
#308=STYLED_ITEM('',(#17959),#318);
#309=STYLED_ITEM('',(#17966),#319);
#310=STYLED_ITEM('',(#17959),#320);
#311=STYLED_ITEM('',(#17987),#321);
#312=STYLED_ITEM('',(#17959),#322);
#313=STYLED_ITEM('',(#17959),#323);
#314=STYLED_ITEM('',(#17980),#324);
#315=STYLED_ITEM('',(#17987),#325);
#316=STYLED_ITEM('',(#17987),#326);
#317=MANIFOLD_SOLID_BREP('Cap_Screw_01',#9628);
#318=MANIFOLD_SOLID_BREP('Bottom_Plate',#9629);
#319=MANIFOLD_SOLID_BREP('Moving_Carriage_02',#9630);
#320=MANIFOLD_SOLID_BREP('Top_Plate',#9631);
#321=MANIFOLD_SOLID_BREP('Clamp_02',#9632);
#322=MANIFOLD_SOLID_BREP('Moving_Carriage_01',#9633);
#323=MANIFOLD_SOLID_BREP('Clamp_01',#9634);
#324=MANIFOLD_SOLID_BREP('Cap_Screw_02',#9635);
#325=MANIFOLD_SOLID_BREP('Clamp_03',#9636);
#326=MANIFOLD_SOLID_BREP('Clamp_04',#9637);
#327=CYLINDRICAL_SURFACE('',#9757,9.);
#328=CYLINDRICAL_SURFACE('',#9761,7.5);
#329=CYLINDRICAL_SURFACE('',#9772,0.5);
#330=CYLINDRICAL_SURFACE('',#9774,0.5);
#331=CYLINDRICAL_SURFACE('',#9778,0.5);
#332=CYLINDRICAL_SURFACE('',#9780,0.5);
#333=CYLINDRICAL_SURFACE('',#9794,0.5);
#334=CYLINDRICAL_SURFACE('',#9802,0.5);
#335=CYLINDRICAL_SURFACE('',#9820,0.5);
#336=CYLINDRICAL_SURFACE('',#9825,0.5);
#337=CYLINDRICAL_SURFACE('',#9826,0.5);
#338=CYLINDRICAL_SURFACE('',#9831,0.5);
#339=CYLINDRICAL_SURFACE('',#9832,0.5);
#340=CYLINDRICAL_SURFACE('',#9844,0.5);
#341=CYLINDRICAL_SURFACE('',#9845,0.5);
#342=CYLINDRICAL_SURFACE('',#9857,0.5);
#343=CYLINDRICAL_SURFACE('',#9858,0.5);
#344=CYLINDRICAL_SURFACE('',#9867,0.5);
#345=CYLINDRICAL_SURFACE('',#9872,0.5);
#346=CYLINDRICAL_SURFACE('',#9873,0.5);
#347=CYLINDRICAL_SURFACE('',#9877,0.5);
#348=CYLINDRICAL_SURFACE('',#9878,0.5);
#349=CYLINDRICAL_SURFACE('',#9886,0.5);
#350=CYLINDRICAL_SURFACE('',#9895,0.5);
#351=CYLINDRICAL_SURFACE('',#9900,0.5);
#352=CYLINDRICAL_SURFACE('',#9901,0.5);
#353=CYLINDRICAL_SURFACE('',#9906,0.5);
#354=CYLINDRICAL_SURFACE('',#9907,0.5);
#355=CYLINDRICAL_SURFACE('',#9908,0.5);
#356=CYLINDRICAL_SURFACE('',#9909,0.5);
#357=CYLINDRICAL_SURFACE('',#9910,0.5);
#358=CYLINDRICAL_SURFACE('',#9911,0.5);
#359=CYLINDRICAL_SURFACE('',#9912,0.5);
#360=CYLINDRICAL_SURFACE('',#9913,0.5);
#361=CYLINDRICAL_SURFACE('',#9914,0.5);
#362=CYLINDRICAL_SURFACE('',#9915,0.5);
#363=CYLINDRICAL_SURFACE('',#9916,0.5);
#364=CYLINDRICAL_SURFACE('',#9917,0.5);
#365=CYLINDRICAL_SURFACE('',#9918,0.5);
#366=CYLINDRICAL_SURFACE('',#9919,0.5);
#367=CYLINDRICAL_SURFACE('',#9920,0.5);
#368=CYLINDRICAL_SURFACE('',#9933,6.);
#369=CYLINDRICAL_SURFACE('',#9936,6.);
#370=CYLINDRICAL_SURFACE('',#9940,6.);
#371=CYLINDRICAL_SURFACE('',#9944,6.);
#372=CYLINDRICAL_SURFACE('',#9960,0.5);
#373=CYLINDRICAL_SURFACE('',#9976,0.5);
#374=CYLINDRICAL_SURFACE('',#9981,0.5);
#375=CYLINDRICAL_SURFACE('',#9986,0.5);
#376=CYLINDRICAL_SURFACE('',#9995,0.5);
#377=CYLINDRICAL_SURFACE('',#10000,0.5);
#378=CYLINDRICAL_SURFACE('',#10005,0.5);
#379=CYLINDRICAL_SURFACE('',#10014,0.5);
#380=CYLINDRICAL_SURFACE('',#10020,0.5);
#381=CYLINDRICAL_SURFACE('',#10038,0.5);
#382=CYLINDRICAL_SURFACE('',#10056,0.5);
#383=CYLINDRICAL_SURFACE('',#10057,0.5);
#384=CYLINDRICAL_SURFACE('',#10063,0.5);
#385=CYLINDRICAL_SURFACE('',#10064,0.5);
#386=CYLINDRICAL_SURFACE('',#10065,0.5);
#387=CYLINDRICAL_SURFACE('',#10066,0.5);
#388=CYLINDRICAL_SURFACE('',#10067,0.5);
#389=CYLINDRICAL_SURFACE('',#10068,0.5);
#390=CYLINDRICAL_SURFACE('',#10069,0.5);
#391=CYLINDRICAL_SURFACE('',#10070,0.5);
#392=CYLINDRICAL_SURFACE('',#10071,0.5);
#393=CYLINDRICAL_SURFACE('',#10072,0.5);
#394=CYLINDRICAL_SURFACE('',#10073,0.5);
#395=CYLINDRICAL_SURFACE('',#10074,0.5);
#396=CYLINDRICAL_SURFACE('',#10075,0.5);
#397=CYLINDRICAL_SURFACE('',#10076,0.5);
#398=CYLINDRICAL_SURFACE('',#10077,0.5);
#399=CYLINDRICAL_SURFACE('',#10078,0.5);
#400=CYLINDRICAL_SURFACE('',#10079,0.5);
#401=CYLINDRICAL_SURFACE('',#10080,0.5);
#402=CYLINDRICAL_SURFACE('',#10081,0.5);
#403=CYLINDRICAL_SURFACE('',#10082,0.5);
#404=CYLINDRICAL_SURFACE('',#10083,0.5);
#405=CYLINDRICAL_SURFACE('',#10084,0.5);
#406=CYLINDRICAL_SURFACE('',#10085,0.5);
#407=CYLINDRICAL_SURFACE('',#10086,0.5);
#408=CYLINDRICAL_SURFACE('',#10102,4.);
#409=CYLINDRICAL_SURFACE('',#10106,4.);
#410=CYLINDRICAL_SURFACE('',#10110,4.);
#411=CYLINDRICAL_SURFACE('',#10114,4.);
#412=CYLINDRICAL_SURFACE('',#10118,4.);
#413=CYLINDRICAL_SURFACE('',#10122,4.);
#414=CYLINDRICAL_SURFACE('',#10126,4.);
#415=CYLINDRICAL_SURFACE('',#10130,4.);
#416=CYLINDRICAL_SURFACE('',#10141,0.5);
#417=CYLINDRICAL_SURFACE('',#10143,0.5);
#418=CYLINDRICAL_SURFACE('',#10147,0.5);
#419=CYLINDRICAL_SURFACE('',#10149,0.5);
#420=CYLINDRICAL_SURFACE('',#10163,0.5);
#421=CYLINDRICAL_SURFACE('',#10171,0.5);
#422=CYLINDRICAL_SURFACE('',#10189,0.5);
#423=CYLINDRICAL_SURFACE('',#10194,0.5);
#424=CYLINDRICAL_SURFACE('',#10195,0.5);
#425=CYLINDRICAL_SURFACE('',#10200,0.5);
#426=CYLINDRICAL_SURFACE('',#10201,0.5);
#427=CYLINDRICAL_SURFACE('',#10213,0.5);
#428=CYLINDRICAL_SURFACE('',#10214,0.5);
#429=CYLINDRICAL_SURFACE('',#10226,0.5);
#430=CYLINDRICAL_SURFACE('',#10227,0.5);
#431=CYLINDRICAL_SURFACE('',#10236,0.5);
#432=CYLINDRICAL_SURFACE('',#10241,0.5);
#433=CYLINDRICAL_SURFACE('',#10242,0.5);
#434=CYLINDRICAL_SURFACE('',#10246,0.5);
#435=CYLINDRICAL_SURFACE('',#10247,0.5);
#436=CYLINDRICAL_SURFACE('',#10255,0.5);
#437=CYLINDRICAL_SURFACE('',#10264,0.5);
#438=CYLINDRICAL_SURFACE('',#10269,0.5);
#439=CYLINDRICAL_SURFACE('',#10270,0.5);
#440=CYLINDRICAL_SURFACE('',#10275,0.5);
#441=CYLINDRICAL_SURFACE('',#10276,0.5);
#442=CYLINDRICAL_SURFACE('',#10277,0.5);
#443=CYLINDRICAL_SURFACE('',#10278,0.5);
#444=CYLINDRICAL_SURFACE('',#10279,0.5);
#445=CYLINDRICAL_SURFACE('',#10280,0.5);
#446=CYLINDRICAL_SURFACE('',#10281,0.5);
#447=CYLINDRICAL_SURFACE('',#10282,0.5);
#448=CYLINDRICAL_SURFACE('',#10283,0.5);
#449=CYLINDRICAL_SURFACE('',#10284,0.5);
#450=CYLINDRICAL_SURFACE('',#10285,0.5);
#451=CYLINDRICAL_SURFACE('',#10286,0.5);
#452=CYLINDRICAL_SURFACE('',#10287,0.5);
#453=CYLINDRICAL_SURFACE('',#10288,0.5);
#454=CYLINDRICAL_SURFACE('',#10289,0.5);
#455=CYLINDRICAL_SURFACE('',#10302,0.3);
#456=CYLINDRICAL_SURFACE('',#10309,0.3);
#457=CYLINDRICAL_SURFACE('',#10314,4.49999999999999);
#458=CYLINDRICAL_SURFACE('',#10332,0.3);
#459=CYLINDRICAL_SURFACE('',#10342,0.3);
#460=CYLINDRICAL_SURFACE('',#10359,0.3);
#461=CYLINDRICAL_SURFACE('',#10364,0.3);
#462=CYLINDRICAL_SURFACE('',#10365,0.3);
#463=CYLINDRICAL_SURFACE('',#10366,0.3);
#464=CYLINDRICAL_SURFACE('',#10367,0.3);
#465=CYLINDRICAL_SURFACE('',#10368,0.3);
#466=CYLINDRICAL_SURFACE('',#10369,0.3);
#467=CYLINDRICAL_SURFACE('',#10370,0.3);
#468=CYLINDRICAL_SURFACE('',#10371,0.3);
#469=CYLINDRICAL_SURFACE('',#10372,0.3);
#470=CYLINDRICAL_SURFACE('',#10373,0.3);
#471=CYLINDRICAL_SURFACE('',#10374,0.3);
#472=CYLINDRICAL_SURFACE('',#10375,0.3);
#473=CYLINDRICAL_SURFACE('',#10376,0.3);
#474=CYLINDRICAL_SURFACE('',#10378,0.3);
#475=CYLINDRICAL_SURFACE('',#10387,0.3);
#476=CYLINDRICAL_SURFACE('',#10393,0.3);
#477=CYLINDRICAL_SURFACE('',#10396,4.49999999999998);
#478=CYLINDRICAL_SURFACE('',#10400,12.5);
#479=CYLINDRICAL_SURFACE('',#10403,12.5);
#480=CYLINDRICAL_SURFACE('',#10420,0.5);
#481=CYLINDRICAL_SURFACE('',#10423,0.5);
#482=CYLINDRICAL_SURFACE('',#10425,5.);
#483=CYLINDRICAL_SURFACE('',#10428,5.);
#484=CYLINDRICAL_SURFACE('',#10431,5.);
#485=CYLINDRICAL_SURFACE('',#10434,5.);
#486=CYLINDRICAL_SURFACE('',#10438,12.5);
#487=CYLINDRICAL_SURFACE('',#10441,5.);
#488=CYLINDRICAL_SURFACE('',#10445,5.);
#489=CYLINDRICAL_SURFACE('',#10448,5.);
#490=CYLINDRICAL_SURFACE('',#10452,5.);
#491=CYLINDRICAL_SURFACE('',#10455,5.);
#492=CYLINDRICAL_SURFACE('',#10458,5.);
#493=CYLINDRICAL_SURFACE('',#10461,5.);
#494=CYLINDRICAL_SURFACE('',#10465,5.);
#495=CYLINDRICAL_SURFACE('',#10474,12.5);
#496=CYLINDRICAL_SURFACE('',#10478,5.);
#497=CYLINDRICAL_SURFACE('',#10487,5.);
#498=CYLINDRICAL_SURFACE('',#10496,5.);
#499=CYLINDRICAL_SURFACE('',#10505,5.);
#500=CYLINDRICAL_SURFACE('',#10508,5.);
#501=CYLINDRICAL_SURFACE('',#10511,0.5);
#502=CYLINDRICAL_SURFACE('',#10512,0.5);
#503=CYLINDRICAL_SURFACE('',#10514,0.5);
#504=CYLINDRICAL_SURFACE('',#10515,0.5);
#505=CYLINDRICAL_SURFACE('',#10517,0.5);
#506=CYLINDRICAL_SURFACE('',#10522,0.5);
#507=CYLINDRICAL_SURFACE('',#10523,0.5);
#508=CYLINDRICAL_SURFACE('',#10525,0.5);
#509=CYLINDRICAL_SURFACE('',#10526,0.5);
#510=CYLINDRICAL_SURFACE('',#10528,0.5);
#511=CYLINDRICAL_SURFACE('',#10530,0.5);
#512=CYLINDRICAL_SURFACE('',#10531,0.5);
#513=CYLINDRICAL_SURFACE('',#10533,0.5);
#514=CYLINDRICAL_SURFACE('',#10534,0.5);
#515=CYLINDRICAL_SURFACE('',#10540,0.5);
#516=CYLINDRICAL_SURFACE('',#10542,0.5);
#517=CYLINDRICAL_SURFACE('',#10543,0.5);
#518=CYLINDRICAL_SURFACE('',#10545,0.5);
#519=CYLINDRICAL_SURFACE('',#10546,0.5);
#520=CYLINDRICAL_SURFACE('',#10548,0.5);
#521=CYLINDRICAL_SURFACE('',#10549,0.5);
#522=CYLINDRICAL_SURFACE('',#10551,0.5);
#523=CYLINDRICAL_SURFACE('',#10552,0.5);
#524=CYLINDRICAL_SURFACE('',#10561,0.5);
#525=CYLINDRICAL_SURFACE('',#10563,0.5);
#526=CYLINDRICAL_SURFACE('',#10564,0.5);
#527=CYLINDRICAL_SURFACE('',#10566,0.5);
#528=CYLINDRICAL_SURFACE('',#10568,0.5);
#529=CYLINDRICAL_SURFACE('',#10569,0.5);
#530=CYLINDRICAL_SURFACE('',#10571,0.5);
#531=CYLINDRICAL_SURFACE('',#10572,0.5);
#532=CYLINDRICAL_SURFACE('',#10573,0.5);
#533=CYLINDRICAL_SURFACE('',#10578,0.5);
#534=CYLINDRICAL_SURFACE('',#10579,0.5);
#535=CYLINDRICAL_SURFACE('',#10581,0.5);
#536=CYLINDRICAL_SURFACE('',#10582,0.5);
#537=CYLINDRICAL_SURFACE('',#10595,0.5);
#538=CYLINDRICAL_SURFACE('',#10608,0.5);
#539=CYLINDRICAL_SURFACE('',#10612,0.5);
#540=CYLINDRICAL_SURFACE('',#10617,0.5);
#541=CYLINDRICAL_SURFACE('',#10625,0.5);
#542=CYLINDRICAL_SURFACE('',#10629,0.5);
#543=CYLINDRICAL_SURFACE('',#10634,0.5);
#544=CYLINDRICAL_SURFACE('',#10642,0.5);
#545=CYLINDRICAL_SURFACE('',#10647,0.5);
#546=CYLINDRICAL_SURFACE('',#10663,0.5);
#547=CYLINDRICAL_SURFACE('',#10679,0.5);
#548=CYLINDRICAL_SURFACE('',#10680,0.5);
#549=CYLINDRICAL_SURFACE('',#10685,0.5);
#550=CYLINDRICAL_SURFACE('',#10686,0.5);
#551=CYLINDRICAL_SURFACE('',#10687,0.5);
#552=CYLINDRICAL_SURFACE('',#10688,0.5);
#553=CYLINDRICAL_SURFACE('',#10689,0.5);
#554=CYLINDRICAL_SURFACE('',#10690,0.5);
#555=CYLINDRICAL_SURFACE('',#10691,0.5);
#556=CYLINDRICAL_SURFACE('',#10692,0.5);
#557=CYLINDRICAL_SURFACE('',#10693,0.5);
#558=CYLINDRICAL_SURFACE('',#10694,0.5);
#559=CYLINDRICAL_SURFACE('',#10695,0.5);
#560=CYLINDRICAL_SURFACE('',#10696,0.5);
#561=CYLINDRICAL_SURFACE('',#10697,0.5);
#562=CYLINDRICAL_SURFACE('',#10698,0.5);
#563=CYLINDRICAL_SURFACE('',#10699,0.5);
#564=CYLINDRICAL_SURFACE('',#10700,0.5);
#565=CYLINDRICAL_SURFACE('',#10701,0.5);
#566=CYLINDRICAL_SURFACE('',#10702,0.5);
#567=CYLINDRICAL_SURFACE('',#10703,0.5);
#568=CYLINDRICAL_SURFACE('',#10704,0.5);
#569=CYLINDRICAL_SURFACE('',#10715,0.3);
#570=CYLINDRICAL_SURFACE('',#10722,0.3);
#571=CYLINDRICAL_SURFACE('',#10727,4.49999999999999);
#572=CYLINDRICAL_SURFACE('',#10745,0.3);
#573=CYLINDRICAL_SURFACE('',#10755,0.3);
#574=CYLINDRICAL_SURFACE('',#10772,0.3);
#575=CYLINDRICAL_SURFACE('',#10777,0.3);
#576=CYLINDRICAL_SURFACE('',#10778,0.3);
#577=CYLINDRICAL_SURFACE('',#10779,0.3);
#578=CYLINDRICAL_SURFACE('',#10780,0.3);
#579=CYLINDRICAL_SURFACE('',#10781,0.3);
#580=CYLINDRICAL_SURFACE('',#10782,0.3);
#581=CYLINDRICAL_SURFACE('',#10783,0.3);
#582=CYLINDRICAL_SURFACE('',#10784,0.3);
#583=CYLINDRICAL_SURFACE('',#10785,0.3);
#584=CYLINDRICAL_SURFACE('',#10786,0.3);
#585=CYLINDRICAL_SURFACE('',#10787,0.3);
#586=CYLINDRICAL_SURFACE('',#10788,0.3);
#587=CYLINDRICAL_SURFACE('',#10789,0.3);
#588=CYLINDRICAL_SURFACE('',#10791,0.3);
#589=CYLINDRICAL_SURFACE('',#10800,0.3);
#590=CYLINDRICAL_SURFACE('',#10806,0.3);
#591=CYLINDRICAL_SURFACE('',#10809,4.49999999999998);
#592=CYLINDRICAL_SURFACE('',#10819,9.);
#593=CYLINDRICAL_SURFACE('',#10823,7.5);
#594=CYLINDRICAL_SURFACE('',#10827,0.3);
#595=CYLINDRICAL_SURFACE('',#10834,0.3);
#596=CYLINDRICAL_SURFACE('',#10839,4.49999999999999);
#597=CYLINDRICAL_SURFACE('',#10857,0.3);
#598=CYLINDRICAL_SURFACE('',#10867,0.3);
#599=CYLINDRICAL_SURFACE('',#10884,0.3);
#600=CYLINDRICAL_SURFACE('',#10889,0.3);
#601=CYLINDRICAL_SURFACE('',#10890,0.3);
#602=CYLINDRICAL_SURFACE('',#10891,0.3);
#603=CYLINDRICAL_SURFACE('',#10892,0.3);
#604=CYLINDRICAL_SURFACE('',#10893,0.3);
#605=CYLINDRICAL_SURFACE('',#10894,0.3);
#606=CYLINDRICAL_SURFACE('',#10895,0.3);
#607=CYLINDRICAL_SURFACE('',#10896,0.3);
#608=CYLINDRICAL_SURFACE('',#10897,0.3);
#609=CYLINDRICAL_SURFACE('',#10898,0.3);
#610=CYLINDRICAL_SURFACE('',#10899,0.3);
#611=CYLINDRICAL_SURFACE('',#10900,0.3);
#612=CYLINDRICAL_SURFACE('',#10901,0.3);
#613=CYLINDRICAL_SURFACE('',#10903,0.3);
#614=CYLINDRICAL_SURFACE('',#10912,0.3);
#615=CYLINDRICAL_SURFACE('',#10918,0.3);
#616=CYLINDRICAL_SURFACE('',#10921,4.49999999999998);
#617=CYLINDRICAL_SURFACE('',#10925,0.3);
#618=CYLINDRICAL_SURFACE('',#10932,0.3);
#619=CYLINDRICAL_SURFACE('',#10937,4.49999999999999);
#620=CYLINDRICAL_SURFACE('',#10955,0.3);
#621=CYLINDRICAL_SURFACE('',#10965,0.3);
#622=CYLINDRICAL_SURFACE('',#10982,0.3);
#623=CYLINDRICAL_SURFACE('',#10987,0.3);
#624=CYLINDRICAL_SURFACE('',#10988,0.3);
#625=CYLINDRICAL_SURFACE('',#10989,0.3);
#626=CYLINDRICAL_SURFACE('',#10990,0.3);
#627=CYLINDRICAL_SURFACE('',#10991,0.3);
#628=CYLINDRICAL_SURFACE('',#10992,0.3);
#629=CYLINDRICAL_SURFACE('',#10993,0.3);
#630=CYLINDRICAL_SURFACE('',#10994,0.3);
#631=CYLINDRICAL_SURFACE('',#10995,0.3);
#632=CYLINDRICAL_SURFACE('',#10996,0.3);
#633=CYLINDRICAL_SURFACE('',#10997,0.3);
#634=CYLINDRICAL_SURFACE('',#10998,0.3);
#635=CYLINDRICAL_SURFACE('',#10999,0.3);
#636=CYLINDRICAL_SURFACE('',#11001,0.3);
#637=CYLINDRICAL_SURFACE('',#11010,0.3);
#638=CYLINDRICAL_SURFACE('',#11016,0.3);
#639=CYLINDRICAL_SURFACE('',#11019,4.49999999999998);
#640=LINE('',#14274,#1305);
#641=LINE('',#14278,#1306);
#642=LINE('',#14282,#1307);
#643=LINE('',#14285,#1308);
#644=LINE('',#14294,#1309);
#645=LINE('',#14296,#1310);
#646=LINE('',#14298,#1311);
#647=LINE('',#14301,#1312);
#648=LINE('',#14307,#1313);
#649=LINE('',#14311,#1314);
#650=LINE('',#14313,#1315);
#651=LINE('',#14314,#1316);
#652=LINE('',#14316,#1317);
#653=LINE('',#14317,#1318);
#654=LINE('',#14320,#1319);
#655=LINE('',#14323,#1320);
#656=LINE('',#14326,#1321);
#657=LINE('',#14329,#1322);
#658=LINE('',#14332,#1323);
#659=LINE('',#14333,#1324);
#660=LINE('',#14336,#1325);
#661=LINE('',#14337,#1326);
#662=LINE('',#14341,#1327);
#663=LINE('',#14344,#1328);
#664=LINE('',#14348,#1329);
#665=LINE('',#14350,#1330);
#666=LINE('',#14352,#1331);
#667=LINE('',#14354,#1332);
#668=LINE('',#14356,#1333);
#669=LINE('',#14358,#1334);
#670=LINE('',#14360,#1335);
#671=LINE('',#14362,#1336);
#672=LINE('',#14366,#1337);
#673=LINE('',#14368,#1338);
#674=LINE('',#14372,#1339);
#675=LINE('',#14376,#1340);
#676=LINE('',#14378,#1341);
#677=LINE('',#14382,#1342);
#678=LINE('',#14383,#1343);
#679=LINE('',#14388,#1344);
#680=LINE('',#14390,#1345);
#681=LINE('',#14393,#1346);
#682=LINE('',#14398,#1347);
#683=LINE('',#14402,#1348);
#684=LINE('',#14403,#1349);
#685=LINE('',#14405,#1350);
#686=LINE('',#14408,#1351);
#687=LINE('',#14412,#1352);
#688=LINE('',#14414,#1353);
#689=LINE('',#14418,#1354);
#690=LINE('',#14420,#1355);
#691=LINE('',#14424,#1356);
#692=LINE('',#14428,#1357);
#693=LINE('',#14430,#1358);
#694=LINE('',#14434,#1359);
#695=LINE('',#14436,#1360);
#696=LINE('',#14437,#1361);
#697=LINE('',#14439,#1362);
#698=LINE('',#14440,#1363);
#699=LINE('',#14443,#1364);
#700=LINE('',#14444,#1365);
#701=LINE('',#14447,#1366);
#702=LINE('',#14474,#1367);
#703=LINE('',#14482,#1368);
#704=LINE('',#14484,#1369);
#705=LINE('',#14485,#1370);
#706=LINE('',#14493,#1371);
#707=LINE('',#14494,#1372);
#708=LINE('',#14496,#1373);
#709=LINE('',#14514,#1374);
#710=LINE('',#14516,#1375);
#711=LINE('',#14517,#1376);
#712=LINE('',#14535,#1377);
#713=LINE('',#14537,#1378);
#714=LINE('',#14538,#1379);
#715=LINE('',#14552,#1380);
#716=LINE('',#14560,#1381);
#717=LINE('',#14562,#1382);
#718=LINE('',#14563,#1383);
#719=LINE('',#14569,#1384);
#720=LINE('',#14570,#1385);
#721=LINE('',#14572,#1386);
#722=LINE('',#14584,#1387);
#723=LINE('',#14604,#1388);
#724=LINE('',#14606,#1389);
#725=LINE('',#14614,#1390);
#726=LINE('',#14615,#1391);
#727=LINE('',#14617,#1392);
#728=LINE('',#14619,#1393);
#729=LINE('',#14621,#1394);
#730=LINE('',#14623,#1395);
#731=LINE('',#14625,#1396);
#732=LINE('',#14626,#1397);
#733=LINE('',#14628,#1398);
#734=LINE('',#14630,#1399);
#735=LINE('',#14632,#1400);
#736=LINE('',#14634,#1401);
#737=LINE('',#14636,#1402);
#738=LINE('',#14638,#1403);
#739=LINE('',#14640,#1404);
#740=LINE('',#14642,#1405);
#741=LINE('',#14644,#1406);
#742=LINE('',#14645,#1407);
#743=LINE('',#14662,#1408);
#744=LINE('',#14668,#1409);
#745=LINE('',#14675,#1410);
#746=LINE('',#14682,#1411);
#747=LINE('',#14708,#1412);
#748=LINE('',#14709,#1413);
#749=LINE('',#14738,#1414);
#750=LINE('',#14739,#1415);
#751=LINE('',#14748,#1416);
#752=LINE('',#14749,#1417);
#753=LINE('',#14758,#1418);
#754=LINE('',#14759,#1419);
#755=LINE('',#14775,#1420);
#756=LINE('',#14776,#1421);
#757=LINE('',#14785,#1422);
#758=LINE('',#14786,#1423);
#759=LINE('',#14795,#1424);
#760=LINE('',#14796,#1425);
#761=LINE('',#14812,#1426);
#762=LINE('',#14813,#1427);
#763=LINE('',#14824,#1428);
#764=LINE('',#14825,#1429);
#765=LINE('',#14857,#1430);
#766=LINE('',#14858,#1431);
#767=LINE('',#14890,#1432);
#768=LINE('',#14891,#1433);
#769=LINE('',#14893,#1434);
#770=LINE('',#14894,#1435);
#771=LINE('',#14905,#1436);
#772=LINE('',#14906,#1437);
#773=LINE('',#14908,#1438);
#774=LINE('',#14909,#1439);
#775=LINE('',#14911,#1440);
#776=LINE('',#14912,#1441);
#777=LINE('',#14914,#1442);
#778=LINE('',#14915,#1443);
#779=LINE('',#14917,#1444);
#780=LINE('',#14918,#1445);
#781=LINE('',#14920,#1446);
#782=LINE('',#14921,#1447);
#783=LINE('',#14923,#1448);
#784=LINE('',#14924,#1449);
#785=LINE('',#14926,#1450);
#786=LINE('',#14927,#1451);
#787=LINE('',#14929,#1452);
#788=LINE('',#14930,#1453);
#789=LINE('',#14932,#1454);
#790=LINE('',#14933,#1455);
#791=LINE('',#14935,#1456);
#792=LINE('',#14936,#1457);
#793=LINE('',#14938,#1458);
#794=LINE('',#14939,#1459);
#795=LINE('',#14941,#1460);
#796=LINE('',#14942,#1461);
#797=LINE('',#14944,#1462);
#798=LINE('',#14945,#1463);
#799=LINE('',#14947,#1464);
#800=LINE('',#14948,#1465);
#801=LINE('',#14950,#1466);
#802=LINE('',#14951,#1467);
#803=LINE('',#14953,#1468);
#804=LINE('',#14954,#1469);
#805=LINE('',#14956,#1470);
#806=LINE('',#14957,#1471);
#807=LINE('',#14959,#1472);
#808=LINE('',#14960,#1473);
#809=LINE('',#14962,#1474);
#810=LINE('',#14963,#1475);
#811=LINE('',#14965,#1476);
#812=LINE('',#14966,#1477);
#813=LINE('',#14968,#1478);
#814=LINE('',#14969,#1479);
#815=LINE('',#14971,#1480);
#816=LINE('',#14972,#1481);
#817=LINE('',#14974,#1482);
#818=LINE('',#14975,#1483);
#819=LINE('',#14995,#1484);
#820=LINE('',#15002,#1485);
#821=LINE('',#15009,#1486);
#822=LINE('',#15016,#1487);
#823=LINE('',#15023,#1488);
#824=LINE('',#15030,#1489);
#825=LINE('',#15037,#1490);
#826=LINE('',#15044,#1491);
#827=LINE('',#15052,#1492);
#828=LINE('',#15054,#1493);
#829=LINE('',#15056,#1494);
#830=LINE('',#15059,#1495);
#831=LINE('',#15065,#1496);
#832=LINE('',#15069,#1497);
#833=LINE('',#15071,#1498);
#834=LINE('',#15072,#1499);
#835=LINE('',#15074,#1500);
#836=LINE('',#15075,#1501);
#837=LINE('',#15078,#1502);
#838=LINE('',#15081,#1503);
#839=LINE('',#15084,#1504);
#840=LINE('',#15087,#1505);
#841=LINE('',#15090,#1506);
#842=LINE('',#15091,#1507);
#843=LINE('',#15094,#1508);
#844=LINE('',#15095,#1509);
#845=LINE('',#15099,#1510);
#846=LINE('',#15102,#1511);
#847=LINE('',#15106,#1512);
#848=LINE('',#15108,#1513);
#849=LINE('',#15110,#1514);
#850=LINE('',#15112,#1515);
#851=LINE('',#15114,#1516);
#852=LINE('',#15116,#1517);
#853=LINE('',#15118,#1518);
#854=LINE('',#15120,#1519);
#855=LINE('',#15124,#1520);
#856=LINE('',#15126,#1521);
#857=LINE('',#15130,#1522);
#858=LINE('',#15134,#1523);
#859=LINE('',#15136,#1524);
#860=LINE('',#15140,#1525);
#861=LINE('',#15141,#1526);
#862=LINE('',#15146,#1527);
#863=LINE('',#15148,#1528);
#864=LINE('',#15151,#1529);
#865=LINE('',#15156,#1530);
#866=LINE('',#15160,#1531);
#867=LINE('',#15161,#1532);
#868=LINE('',#15163,#1533);
#869=LINE('',#15166,#1534);
#870=LINE('',#15170,#1535);
#871=LINE('',#15172,#1536);
#872=LINE('',#15176,#1537);
#873=LINE('',#15178,#1538);
#874=LINE('',#15182,#1539);
#875=LINE('',#15186,#1540);
#876=LINE('',#15188,#1541);
#877=LINE('',#15192,#1542);
#878=LINE('',#15194,#1543);
#879=LINE('',#15195,#1544);
#880=LINE('',#15197,#1545);
#881=LINE('',#15198,#1546);
#882=LINE('',#15201,#1547);
#883=LINE('',#15202,#1548);
#884=LINE('',#15205,#1549);
#885=LINE('',#15232,#1550);
#886=LINE('',#15240,#1551);
#887=LINE('',#15242,#1552);
#888=LINE('',#15243,#1553);
#889=LINE('',#15251,#1554);
#890=LINE('',#15252,#1555);
#891=LINE('',#15254,#1556);
#892=LINE('',#15272,#1557);
#893=LINE('',#15274,#1558);
#894=LINE('',#15275,#1559);
#895=LINE('',#15293,#1560);
#896=LINE('',#15295,#1561);
#897=LINE('',#15296,#1562);
#898=LINE('',#15310,#1563);
#899=LINE('',#15318,#1564);
#900=LINE('',#15320,#1565);
#901=LINE('',#15321,#1566);
#902=LINE('',#15327,#1567);
#903=LINE('',#15328,#1568);
#904=LINE('',#15330,#1569);
#905=LINE('',#15342,#1570);
#906=LINE('',#15362,#1571);
#907=LINE('',#15364,#1572);
#908=LINE('',#15372,#1573);
#909=LINE('',#15373,#1574);
#910=LINE('',#15375,#1575);
#911=LINE('',#15377,#1576);
#912=LINE('',#15379,#1577);
#913=LINE('',#15381,#1578);
#914=LINE('',#15383,#1579);
#915=LINE('',#15384,#1580);
#916=LINE('',#15386,#1581);
#917=LINE('',#15388,#1582);
#918=LINE('',#15390,#1583);
#919=LINE('',#15392,#1584);
#920=LINE('',#15394,#1585);
#921=LINE('',#15396,#1586);
#922=LINE('',#15398,#1587);
#923=LINE('',#15400,#1588);
#924=LINE('',#15402,#1589);
#925=LINE('',#15403,#1590);
#926=LINE('',#15421,#1591);
#927=LINE('',#15424,#1592);
#928=LINE('',#15435,#1593);
#929=LINE('',#15436,#1594);
#930=LINE('',#15442,#1595);
#931=LINE('',#15445,#1596);
#932=LINE('',#15448,#1597);
#933=LINE('',#15449,#1598);
#934=LINE('',#15453,#1599);
#935=LINE('',#15455,#1600);
#936=LINE('',#15457,#1601);
#937=LINE('',#15458,#1602);
#938=LINE('',#15484,#1603);
#939=LINE('',#15487,#1604);
#940=LINE('',#15502,#1605);
#941=LINE('',#15503,#1606);
#942=LINE('',#15532,#1607);
#943=LINE('',#15533,#1608);
#944=LINE('',#15542,#1609);
#945=LINE('',#15543,#1610);
#946=LINE('',#15545,#1611);
#947=LINE('',#15546,#1612);
#948=LINE('',#15548,#1613);
#949=LINE('',#15549,#1614);
#950=LINE('',#15551,#1615);
#951=LINE('',#15552,#1616);
#952=LINE('',#15554,#1617);
#953=LINE('',#15555,#1618);
#954=LINE('',#15557,#1619);
#955=LINE('',#15558,#1620);
#956=LINE('',#15560,#1621);
#957=LINE('',#15562,#1622);
#958=LINE('',#15564,#1623);
#959=LINE('',#15565,#1624);
#960=LINE('',#15567,#1625);
#961=LINE('',#15568,#1626);
#962=LINE('',#15570,#1627);
#963=LINE('',#15572,#1628);
#964=LINE('',#15575,#1629);
#965=LINE('',#15578,#1630);
#966=LINE('',#15580,#1631);
#967=LINE('',#15581,#1632);
#968=LINE('',#15583,#1633);
#969=LINE('',#15589,#1634);
#970=LINE('',#15593,#1635);
#971=LINE('',#15606,#1636);
#972=LINE('',#15609,#1637);
#973=LINE('',#15617,#1638);
#974=LINE('',#15623,#1639);
#975=LINE('',#15638,#1640);
#976=LINE('',#15664,#1641);
#977=LINE('',#15679,#1642);
#978=LINE('',#15681,#1643);
#979=LINE('',#15683,#1644);
#980=LINE('',#15687,#1645);
#981=LINE('',#15691,#1646);
#982=LINE('',#15695,#1647);
#983=LINE('',#15699,#1648);
#984=LINE('',#15701,#1649);
#985=LINE('',#15703,#1650);
#986=LINE('',#15707,#1651);
#987=LINE('',#15713,#1652);
#988=LINE('',#15719,#1653);
#989=LINE('',#15724,#1654);
#990=LINE('',#15727,#1655);
#991=LINE('',#15731,#1656);
#992=LINE('',#15732,#1657);
#993=LINE('',#15735,#1658);
#994=LINE('',#15740,#1659);
#995=LINE('',#15753,#1660);
#996=LINE('',#15779,#1661);
#997=LINE('',#15794,#1662);
#998=LINE('',#15800,#1663);
#999=LINE('',#15806,#1664);
#1000=LINE('',#15821,#1665);
#1001=LINE('',#15844,#1666);
#1002=LINE('',#15861,#1667);
#1003=LINE('',#15867,#1668);
#1004=LINE('',#15882,#1669);
#1005=LINE('',#15905,#1670);
#1006=LINE('',#15922,#1671);
#1007=LINE('',#15928,#1672);
#1008=LINE('',#15943,#1673);
#1009=LINE('',#15966,#1674);
#1010=LINE('',#15983,#1675);
#1011=LINE('',#15988,#1676);
#1012=LINE('',#16001,#1677);
#1013=LINE('',#16027,#1678);
#1014=LINE('',#16042,#1679);
#1015=LINE('',#16048,#1680);
#1016=LINE('',#16063,#1681);
#1017=LINE('',#16086,#1682);
#1018=LINE('',#16103,#1683);
#1019=LINE('',#16118,#1684);
#1020=LINE('',#16144,#1685);
#1021=LINE('',#16247,#1686);
#1022=LINE('',#16262,#1687);
#1023=LINE('',#16285,#1688);
#1024=LINE('',#16302,#1689);
#1025=LINE('',#16317,#1690);
#1026=LINE('',#16343,#1691);
#1027=LINE('',#16446,#1692);
#1028=LINE('',#16461,#1693);
#1029=LINE('',#16487,#1694);
#1030=LINE('',#16590,#1695);
#1031=LINE('',#16605,#1696);
#1032=LINE('',#16631,#1697);
#1033=LINE('',#16734,#1698);
#1034=LINE('',#16739,#1699);
#1035=LINE('',#16752,#1700);
#1036=LINE('',#16778,#1701);
#1037=LINE('',#16790,#1702);
#1038=LINE('',#16794,#1703);
#1039=LINE('',#16796,#1704);
#1040=LINE('',#16799,#1705);
#1041=LINE('',#16802,#1706);
#1042=LINE('',#16805,#1707);
#1043=LINE('',#16806,#1708);
#1044=LINE('',#16808,#1709);
#1045=LINE('',#16811,#1710);
#1046=LINE('',#16812,#1711);
#1047=LINE('',#16814,#1712);
#1048=LINE('',#16816,#1713);
#1049=LINE('',#16820,#1714);
#1050=LINE('',#16822,#1715);
#1051=LINE('',#16825,#1716);
#1052=LINE('',#16829,#1717);
#1053=LINE('',#16832,#1718);
#1054=LINE('',#16834,#1719);
#1055=LINE('',#16835,#1720);
#1056=LINE('',#16838,#1721);
#1057=LINE('',#16841,#1722);
#1058=LINE('',#16843,#1723);
#1059=LINE('',#16844,#1724);
#1060=LINE('',#16846,#1725);
#1061=LINE('',#16847,#1726);
#1062=LINE('',#16850,#1727);
#1063=LINE('',#16851,#1728);
#1064=LINE('',#16853,#1729);
#1065=LINE('',#16856,#1730);
#1066=LINE('',#16857,#1731);
#1067=LINE('',#16859,#1732);
#1068=LINE('',#16861,#1733);
#1069=LINE('',#16864,#1734);
#1070=LINE('',#16867,#1735);
#1071=LINE('',#16869,#1736);
#1072=LINE('',#16870,#1737);
#1073=LINE('',#16873,#1738);
#1074=LINE('',#16876,#1739);
#1075=LINE('',#16878,#1740);
#1076=LINE('',#16879,#1741);
#1077=LINE('',#16883,#1742);
#1078=LINE('',#16885,#1743);
#1079=LINE('',#16888,#1744);
#1080=LINE('',#16891,#1745);
#1081=LINE('',#16893,#1746);
#1082=LINE('',#16896,#1747);
#1083=LINE('',#16897,#1748);
#1084=LINE('',#16899,#1749);
#1085=LINE('',#16902,#1750);
#1086=LINE('',#16903,#1751);
#1087=LINE('',#16905,#1752);
#1088=LINE('',#16908,#1753);
#1089=LINE('',#16909,#1754);
#1090=LINE('',#16912,#1755);
#1091=LINE('',#16913,#1756);
#1092=LINE('',#16915,#1757);
#1093=LINE('',#16917,#1758);
#1094=LINE('',#16925,#1759);
#1095=LINE('',#16926,#1760);
#1096=LINE('',#16927,#1761);
#1097=LINE('',#16928,#1762);
#1098=LINE('',#16930,#1763);
#1099=LINE('',#16932,#1764);
#1100=LINE('',#16934,#1765);
#1101=LINE('',#16935,#1766);
#1102=LINE('',#16937,#1767);
#1103=LINE('',#16940,#1768);
#1104=LINE('',#16943,#1769);
#1105=LINE('',#16945,#1770);
#1106=LINE('',#16947,#1771);
#1107=LINE('',#16950,#1772);
#1108=LINE('',#16951,#1773);
#1109=LINE('',#16953,#1774);
#1110=LINE('',#16955,#1775);
#1111=LINE('',#16957,#1776);
#1112=LINE('',#16964,#1777);
#1113=LINE('',#16965,#1778);
#1114=LINE('',#16966,#1779);
#1115=LINE('',#16968,#1780);
#1116=LINE('',#16970,#1781);
#1117=LINE('',#16972,#1782);
#1118=LINE('',#16973,#1783);
#1119=LINE('',#16989,#1784);
#1120=LINE('',#17009,#1785);
#1121=LINE('',#17015,#1786);
#1122=LINE('',#17023,#1787);
#1123=LINE('',#17035,#1788);
#1124=LINE('',#17041,#1789);
#1125=LINE('',#17050,#1790);
#1126=LINE('',#17051,#1791);
#1127=LINE('',#17064,#1792);
#1128=LINE('',#17065,#1793);
#1129=LINE('',#17073,#1794);
#1130=LINE('',#17099,#1795);
#1131=LINE('',#17123,#1796);
#1132=LINE('',#17125,#1797);
#1133=LINE('',#17133,#1798);
#1134=LINE('',#17135,#1799);
#1135=LINE('',#17137,#1800);
#1136=LINE('',#17139,#1801);
#1137=LINE('',#17140,#1802);
#1138=LINE('',#17142,#1803);
#1139=LINE('',#17144,#1804);
#1140=LINE('',#17146,#1805);
#1141=LINE('',#17147,#1806);
#1142=LINE('',#17149,#1807);
#1143=LINE('',#17150,#1808);
#1144=LINE('',#17152,#1809);
#1145=LINE('',#17153,#1810);
#1146=LINE('',#17155,#1811);
#1147=LINE('',#17157,#1812);
#1148=LINE('',#17158,#1813);
#1149=LINE('',#17160,#1814);
#1150=LINE('',#17161,#1815);
#1151=LINE('',#17163,#1816);
#1152=LINE('',#17165,#1817);
#1153=LINE('',#17167,#1818);
#1154=LINE('',#17169,#1819);
#1155=LINE('',#17171,#1820);
#1156=LINE('',#17173,#1821);
#1157=LINE('',#17175,#1822);
#1158=LINE('',#17177,#1823);
#1159=LINE('',#17178,#1824);
#1160=LINE('',#17194,#1825);
#1161=LINE('',#17197,#1826);
#1162=LINE('',#17208,#1827);
#1163=LINE('',#17209,#1828);
#1164=LINE('',#17215,#1829);
#1165=LINE('',#17218,#1830);
#1166=LINE('',#17221,#1831);
#1167=LINE('',#17222,#1832);
#1168=LINE('',#17226,#1833);
#1169=LINE('',#17228,#1834);
#1170=LINE('',#17230,#1835);
#1171=LINE('',#17231,#1836);
#1172=LINE('',#17257,#1837);
#1173=LINE('',#17259,#1838);
#1174=LINE('',#17275,#1839);
#1175=LINE('',#17276,#1840);
#1176=LINE('',#17305,#1841);
#1177=LINE('',#17306,#1842);
#1178=LINE('',#17315,#1843);
#1179=LINE('',#17316,#1844);
#1180=LINE('',#17318,#1845);
#1181=LINE('',#17319,#1846);
#1182=LINE('',#17321,#1847);
#1183=LINE('',#17322,#1848);
#1184=LINE('',#17324,#1849);
#1185=LINE('',#17325,#1850);
#1186=LINE('',#17327,#1851);
#1187=LINE('',#17328,#1852);
#1188=LINE('',#17330,#1853);
#1189=LINE('',#17331,#1854);
#1190=LINE('',#17333,#1855);
#1191=LINE('',#17335,#1856);
#1192=LINE('',#17337,#1857);
#1193=LINE('',#17338,#1858);
#1194=LINE('',#17340,#1859);
#1195=LINE('',#17341,#1860);
#1196=LINE('',#17343,#1861);
#1197=LINE('',#17345,#1862);
#1198=LINE('',#17348,#1863);
#1199=LINE('',#17350,#1864);
#1200=LINE('',#17353,#1865);
#1201=LINE('',#17354,#1866);
#1202=LINE('',#17356,#1867);
#1203=LINE('',#17362,#1868);
#1204=LINE('',#17366,#1869);
#1205=LINE('',#17379,#1870);
#1206=LINE('',#17382,#1871);
#1207=LINE('',#17395,#1872);
#1208=LINE('',#17399,#1873);
#1209=LINE('',#17403,#1874);
#1210=LINE('',#17406,#1875);
#1211=LINE('',#17415,#1876);
#1212=LINE('',#17418,#1877);
#1213=LINE('',#17429,#1878);
#1214=LINE('',#17430,#1879);
#1215=LINE('',#17436,#1880);
#1216=LINE('',#17439,#1881);
#1217=LINE('',#17442,#1882);
#1218=LINE('',#17443,#1883);
#1219=LINE('',#17447,#1884);
#1220=LINE('',#17449,#1885);
#1221=LINE('',#17451,#1886);
#1222=LINE('',#17452,#1887);
#1223=LINE('',#17478,#1888);
#1224=LINE('',#17481,#1889);
#1225=LINE('',#17496,#1890);
#1226=LINE('',#17497,#1891);
#1227=LINE('',#17526,#1892);
#1228=LINE('',#17527,#1893);
#1229=LINE('',#17536,#1894);
#1230=LINE('',#17537,#1895);
#1231=LINE('',#17539,#1896);
#1232=LINE('',#17540,#1897);
#1233=LINE('',#17542,#1898);
#1234=LINE('',#17543,#1899);
#1235=LINE('',#17545,#1900);
#1236=LINE('',#17546,#1901);
#1237=LINE('',#17548,#1902);
#1238=LINE('',#17549,#1903);
#1239=LINE('',#17551,#1904);
#1240=LINE('',#17552,#1905);
#1241=LINE('',#17554,#1906);
#1242=LINE('',#17556,#1907);
#1243=LINE('',#17558,#1908);
#1244=LINE('',#17559,#1909);
#1245=LINE('',#17561,#1910);
#1246=LINE('',#17562,#1911);
#1247=LINE('',#17564,#1912);
#1248=LINE('',#17566,#1913);
#1249=LINE('',#17569,#1914);
#1250=LINE('',#17572,#1915);
#1251=LINE('',#17574,#1916);
#1252=LINE('',#17575,#1917);
#1253=LINE('',#17577,#1918);
#1254=LINE('',#17583,#1919);
#1255=LINE('',#17587,#1920);
#1256=LINE('',#17600,#1921);
#1257=LINE('',#17603,#1922);
#1258=LINE('',#17612,#1923);
#1259=LINE('',#17615,#1924);
#1260=LINE('',#17626,#1925);
#1261=LINE('',#17627,#1926);
#1262=LINE('',#17633,#1927);
#1263=LINE('',#17636,#1928);
#1264=LINE('',#17639,#1929);
#1265=LINE('',#17640,#1930);
#1266=LINE('',#17644,#1931);
#1267=LINE('',#17646,#1932);
#1268=LINE('',#17648,#1933);
#1269=LINE('',#17649,#1934);
#1270=LINE('',#17675,#1935);
#1271=LINE('',#17677,#1936);
#1272=LINE('',#17693,#1937);
#1273=LINE('',#17694,#1938);
#1274=LINE('',#17723,#1939);
#1275=LINE('',#17724,#1940);
#1276=LINE('',#17733,#1941);
#1277=LINE('',#17734,#1942);
#1278=LINE('',#17736,#1943);
#1279=LINE('',#17737,#1944);
#1280=LINE('',#17739,#1945);
#1281=LINE('',#17740,#1946);
#1282=LINE('',#17742,#1947);
#1283=LINE('',#17743,#1948);
#1284=LINE('',#17745,#1949);
#1285=LINE('',#17746,#1950);
#1286=LINE('',#17748,#1951);
#1287=LINE('',#17749,#1952);
#1288=LINE('',#17751,#1953);
#1289=LINE('',#17753,#1954);
#1290=LINE('',#17755,#1955);
#1291=LINE('',#17756,#1956);
#1292=LINE('',#17758,#1957);
#1293=LINE('',#17759,#1958);
#1294=LINE('',#17761,#1959);
#1295=LINE('',#17763,#1960);
#1296=LINE('',#17766,#1961);
#1297=LINE('',#17768,#1962);
#1298=LINE('',#17771,#1963);
#1299=LINE('',#17772,#1964);
#1300=LINE('',#17774,#1965);
#1301=LINE('',#17780,#1966);
#1302=LINE('',#17784,#1967);
#1303=LINE('',#17797,#1968);
#1304=LINE('',#17800,#1969);
#1305=VECTOR('',#11046,8.5);
#1306=VECTOR('',#11051,9.);
#1307=VECTOR('',#11058,8.5);
#1308=VECTOR('',#11061,7.5);
#1309=VECTOR('',#11072,10.);
#1310=VECTOR('',#11073,10.);
#1311=VECTOR('',#11074,10.);
#1312=VECTOR('',#11077,10.);
#1313=VECTOR('',#11082,10.);
#1314=VECTOR('',#11085,10.);
#1315=VECTOR('',#11086,10.);
#1316=VECTOR('',#11087,10.);
#1317=VECTOR('',#11090,10.);
#1318=VECTOR('',#11091,10.);
#1319=VECTOR('',#11094,10.);
#1320=VECTOR('',#11097,10.);
#1321=VECTOR('',#11100,10.);
#1322=VECTOR('',#11103,10.);
#1323=VECTOR('',#11106,10.);
#1324=VECTOR('',#11107,10.);
#1325=VECTOR('',#11110,10.);
#1326=VECTOR('',#11111,10.);
#1327=VECTOR('',#11116,10.);
#1328=VECTOR('',#11119,10.);
#1329=VECTOR('',#11124,10.);
#1330=VECTOR('',#11125,10.);
#1331=VECTOR('',#11126,10.);
#1332=VECTOR('',#11127,10.);
#1333=VECTOR('',#11128,10.);
#1334=VECTOR('',#11129,10.);
#1335=VECTOR('',#11130,10.);
#1336=VECTOR('',#11131,10.);
#1337=VECTOR('',#11134,10.);
#1338=VECTOR('',#11135,10.);
#1339=VECTOR('',#11138,10.);
#1340=VECTOR('',#11141,10.);
#1341=VECTOR('',#11142,10.);
#1342=VECTOR('',#11145,10.);
#1343=VECTOR('',#11146,10.);
#1344=VECTOR('',#11151,10.);
#1345=VECTOR('',#11152,10.);
#1346=VECTOR('',#11155,10.);
#1347=VECTOR('',#11160,10.);
#1348=VECTOR('',#11163,10.);
#1349=VECTOR('',#11164,10.);
#1350=VECTOR('',#11167,10.);
#1351=VECTOR('',#11170,10.);
#1352=VECTOR('',#11175,10.);
#1353=VECTOR('',#11176,10.);
#1354=VECTOR('',#11179,10.);
#1355=VECTOR('',#11180,10.);
#1356=VECTOR('',#11183,10.);
#1357=VECTOR('',#11186,10.);
#1358=VECTOR('',#11187,10.);
#1359=VECTOR('',#11190,10.);
#1360=VECTOR('',#11191,10.);
#1361=VECTOR('',#11192,10.);
#1362=VECTOR('',#11193,10.);
#1363=VECTOR('',#11194,10.);
#1364=VECTOR('',#11197,10.);
#1365=VECTOR('',#11198,10.);
#1366=VECTOR('',#11201,10.);
#1367=VECTOR('',#11238,10.);
#1368=VECTOR('',#11249,10.);
#1369=VECTOR('',#11252,10.);
#1370=VECTOR('',#11253,10.);
#1371=VECTOR('',#11264,10.);
#1372=VECTOR('',#11265,10.);
#1373=VECTOR('',#11268,10.);
#1374=VECTOR('',#11293,10.);
#1375=VECTOR('',#11296,10.);
#1376=VECTOR('',#11297,10.);
#1377=VECTOR('',#11322,10.);
#1378=VECTOR('',#11325,10.);
#1379=VECTOR('',#11326,10.);
#1380=VECTOR('',#11345,10.);
#1381=VECTOR('',#11356,10.);
#1382=VECTOR('',#11359,10.);
#1383=VECTOR('',#11360,10.);
#1384=VECTOR('',#11369,10.);
#1385=VECTOR('',#11370,10.);
#1386=VECTOR('',#11373,10.);
#1387=VECTOR('',#11390,10.);
#1388=VECTOR('',#11419,10.);
#1389=VECTOR('',#11422,10.);
#1390=VECTOR('',#11433,10.);
#1391=VECTOR('',#11434,10.);
#1392=VECTOR('',#11437,10.);
#1393=VECTOR('',#11440,10.);
#1394=VECTOR('',#11443,10.);
#1395=VECTOR('',#11446,10.);
#1396=VECTOR('',#11449,10.);
#1397=VECTOR('',#11450,10.);
#1398=VECTOR('',#11453,10.);
#1399=VECTOR('',#11456,10.);
#1400=VECTOR('',#11459,10.);
#1401=VECTOR('',#11462,10.);
#1402=VECTOR('',#11465,10.);
#1403=VECTOR('',#11468,10.);
#1404=VECTOR('',#11471,10.);
#1405=VECTOR('',#11474,10.);
#1406=VECTOR('',#11477,10.);
#1407=VECTOR('',#11478,10.);
#1408=VECTOR('',#11507,6.);
#1409=VECTOR('',#11514,6.);
#1410=VECTOR('',#11523,6.);
#1411=VECTOR('',#11532,6.);
#1412=VECTOR('',#11563,10.);
#1413=VECTOR('',#11564,10.);
#1414=VECTOR('',#11597,10.);
#1415=VECTOR('',#11598,10.);
#1416=VECTOR('',#11609,10.);
#1417=VECTOR('',#11610,10.);
#1418=VECTOR('',#11621,10.);
#1419=VECTOR('',#11622,10.);
#1420=VECTOR('',#11641,10.);
#1421=VECTOR('',#11642,10.);
#1422=VECTOR('',#11653,10.);
#1423=VECTOR('',#11654,10.);
#1424=VECTOR('',#11665,10.);
#1425=VECTOR('',#11666,10.);
#1426=VECTOR('',#11685,10.);
#1427=VECTOR('',#11686,10.);
#1428=VECTOR('',#11699,10.);
#1429=VECTOR('',#11700,10.);
#1430=VECTOR('',#11737,10.);
#1431=VECTOR('',#11738,10.);
#1432=VECTOR('',#11775,10.);
#1433=VECTOR('',#11776,10.);
#1434=VECTOR('',#11779,10.);
#1435=VECTOR('',#11780,10.);
#1436=VECTOR('',#11793,10.);
#1437=VECTOR('',#11794,10.);
#1438=VECTOR('',#11797,10.);
#1439=VECTOR('',#11798,10.);
#1440=VECTOR('',#11801,10.);
#1441=VECTOR('',#11802,10.);
#1442=VECTOR('',#11805,10.);
#1443=VECTOR('',#11806,10.);
#1444=VECTOR('',#11809,10.);
#1445=VECTOR('',#11810,10.);
#1446=VECTOR('',#11813,10.);
#1447=VECTOR('',#11814,10.);
#1448=VECTOR('',#11817,10.);
#1449=VECTOR('',#11818,10.);
#1450=VECTOR('',#11821,10.);
#1451=VECTOR('',#11822,10.);
#1452=VECTOR('',#11825,10.);
#1453=VECTOR('',#11826,10.);
#1454=VECTOR('',#11829,10.);
#1455=VECTOR('',#11830,10.);
#1456=VECTOR('',#11833,10.);
#1457=VECTOR('',#11834,10.);
#1458=VECTOR('',#11837,10.);
#1459=VECTOR('',#11838,10.);
#1460=VECTOR('',#11841,10.);
#1461=VECTOR('',#11842,10.);
#1462=VECTOR('',#11845,10.);
#1463=VECTOR('',#11846,10.);
#1464=VECTOR('',#11849,10.);
#1465=VECTOR('',#11850,10.);
#1466=VECTOR('',#11853,10.);
#1467=VECTOR('',#11854,10.);
#1468=VECTOR('',#11857,10.);
#1469=VECTOR('',#11858,10.);
#1470=VECTOR('',#11861,10.);
#1471=VECTOR('',#11862,10.);
#1472=VECTOR('',#11865,10.);
#1473=VECTOR('',#11866,10.);
#1474=VECTOR('',#11869,10.);
#1475=VECTOR('',#11870,10.);
#1476=VECTOR('',#11873,10.);
#1477=VECTOR('',#11874,10.);
#1478=VECTOR('',#11877,10.);
#1479=VECTOR('',#11878,10.);
#1480=VECTOR('',#11881,10.);
#1481=VECTOR('',#11882,10.);
#1482=VECTOR('',#11885,10.);
#1483=VECTOR('',#11886,10.);
#1484=VECTOR('',#11921,4.);
#1485=VECTOR('',#11930,4.);
#1486=VECTOR('',#11939,4.);
#1487=VECTOR('',#11948,4.);
#1488=VECTOR('',#11957,4.);
#1489=VECTOR('',#11966,4.);
#1490=VECTOR('',#11975,4.);
#1491=VECTOR('',#11984,4.);
#1492=VECTOR('',#11993,10.);
#1493=VECTOR('',#11994,10.);
#1494=VECTOR('',#11995,10.);
#1495=VECTOR('',#11998,10.);
#1496=VECTOR('',#12003,10.);
#1497=VECTOR('',#12006,10.);
#1498=VECTOR('',#12007,10.);
#1499=VECTOR('',#12008,10.);
#1500=VECTOR('',#12011,10.);
#1501=VECTOR('',#12012,10.);
#1502=VECTOR('',#12015,10.);
#1503=VECTOR('',#12018,10.);
#1504=VECTOR('',#12021,10.);
#1505=VECTOR('',#12024,10.);
#1506=VECTOR('',#12027,10.);
#1507=VECTOR('',#12028,10.);
#1508=VECTOR('',#12031,10.);
#1509=VECTOR('',#12032,10.);
#1510=VECTOR('',#12037,10.);
#1511=VECTOR('',#12040,10.);
#1512=VECTOR('',#12045,10.);
#1513=VECTOR('',#12046,10.);
#1514=VECTOR('',#12047,10.);
#1515=VECTOR('',#12048,10.);
#1516=VECTOR('',#12049,10.);
#1517=VECTOR('',#12050,10.);
#1518=VECTOR('',#12051,10.);
#1519=VECTOR('',#12052,10.);
#1520=VECTOR('',#12055,10.);
#1521=VECTOR('',#12056,10.);
#1522=VECTOR('',#12059,10.);
#1523=VECTOR('',#12062,10.);
#1524=VECTOR('',#12063,10.);
#1525=VECTOR('',#12066,10.);
#1526=VECTOR('',#12067,10.);
#1527=VECTOR('',#12072,10.);
#1528=VECTOR('',#12073,10.);
#1529=VECTOR('',#12076,10.);
#1530=VECTOR('',#12081,10.);
#1531=VECTOR('',#12084,10.);
#1532=VECTOR('',#12085,10.);
#1533=VECTOR('',#12088,10.);
#1534=VECTOR('',#12091,10.);
#1535=VECTOR('',#12096,10.);
#1536=VECTOR('',#12097,10.);
#1537=VECTOR('',#12100,10.);
#1538=VECTOR('',#12101,10.);
#1539=VECTOR('',#12104,10.);
#1540=VECTOR('',#12107,10.);
#1541=VECTOR('',#12108,10.);
#1542=VECTOR('',#12111,10.);
#1543=VECTOR('',#12112,10.);
#1544=VECTOR('',#12113,10.);
#1545=VECTOR('',#12114,10.);
#1546=VECTOR('',#12115,10.);
#1547=VECTOR('',#12118,10.);
#1548=VECTOR('',#12119,10.);
#1549=VECTOR('',#12122,10.);
#1550=VECTOR('',#12159,10.);
#1551=VECTOR('',#12170,10.);
#1552=VECTOR('',#12173,10.);
#1553=VECTOR('',#12174,10.);
#1554=VECTOR('',#12185,10.);
#1555=VECTOR('',#12186,10.);
#1556=VECTOR('',#12189,10.);
#1557=VECTOR('',#12214,10.);
#1558=VECTOR('',#12217,10.);
#1559=VECTOR('',#12218,10.);
#1560=VECTOR('',#12243,10.);
#1561=VECTOR('',#12246,10.);
#1562=VECTOR('',#12247,10.);
#1563=VECTOR('',#12266,10.);
#1564=VECTOR('',#12277,10.);
#1565=VECTOR('',#12280,10.);
#1566=VECTOR('',#12281,10.);
#1567=VECTOR('',#12290,10.);
#1568=VECTOR('',#12291,10.);
#1569=VECTOR('',#12294,10.);
#1570=VECTOR('',#12311,10.);
#1571=VECTOR('',#12340,10.);
#1572=VECTOR('',#12343,10.);
#1573=VECTOR('',#12354,10.);
#1574=VECTOR('',#12355,10.);
#1575=VECTOR('',#12358,10.);
#1576=VECTOR('',#12361,10.);
#1577=VECTOR('',#12364,10.);
#1578=VECTOR('',#12367,10.);
#1579=VECTOR('',#12370,10.);
#1580=VECTOR('',#12371,10.);
#1581=VECTOR('',#12374,10.);
#1582=VECTOR('',#12377,10.);
#1583=VECTOR('',#12380,10.);
#1584=VECTOR('',#12383,10.);
#1585=VECTOR('',#12386,10.);
#1586=VECTOR('',#12389,10.);
#1587=VECTOR('',#12392,10.);
#1588=VECTOR('',#12395,10.);
#1589=VECTOR('',#12398,10.);
#1590=VECTOR('',#12399,10.);
#1591=VECTOR('',#12428,10.);
#1592=VECTOR('',#12431,10.);
#1593=VECTOR('',#12444,10.);
#1594=VECTOR('',#12445,10.);
#1595=VECTOR('',#12454,10.);
#1596=VECTOR('',#12457,10.);
#1597=VECTOR('',#12460,10.);
#1598=VECTOR('',#12461,10.);
#1599=VECTOR('',#12464,10.);
#1600=VECTOR('',#12465,10.);
#1601=VECTOR('',#12466,10.);
#1602=VECTOR('',#12467,10.);
#1603=VECTOR('',#12498,10.);
#1604=VECTOR('',#12501,10.);
#1605=VECTOR('',#12520,10.);
#1606=VECTOR('',#12521,10.);
#1607=VECTOR('',#12556,10.);
#1608=VECTOR('',#12557,10.);
#1609=VECTOR('',#12568,10.);
#1610=VECTOR('',#12569,10.);
#1611=VECTOR('',#12572,10.);
#1612=VECTOR('',#12573,10.);
#1613=VECTOR('',#12576,10.);
#1614=VECTOR('',#12577,10.);
#1615=VECTOR('',#12580,10.);
#1616=VECTOR('',#12581,10.);
#1617=VECTOR('',#12584,10.);
#1618=VECTOR('',#12585,10.);
#1619=VECTOR('',#12588,10.);
#1620=VECTOR('',#12589,10.);
#1621=VECTOR('',#12592,10.);
#1622=VECTOR('',#12595,10.);
#1623=VECTOR('',#12598,10.);
#1624=VECTOR('',#12599,10.);
#1625=VECTOR('',#12602,10.);
#1626=VECTOR('',#12603,10.);
#1627=VECTOR('',#12606,10.);
#1628=VECTOR('',#12609,10.);
#1629=VECTOR('',#12612,10.);
#1630=VECTOR('',#12615,10.);
#1631=VECTOR('',#12618,10.);
#1632=VECTOR('',#12619,10.);
#1633=VECTOR('',#12622,10.);
#1634=VECTOR('',#12629,10.);
#1635=VECTOR('',#12632,10.);
#1636=VECTOR('',#12655,10.);
#1637=VECTOR('',#12660,10.);
#1638=VECTOR('',#12671,12.5);
#1639=VECTOR('',#12678,12.5);
#1640=VECTOR('',#12681,10.);
#1641=VECTOR('',#12684,10.);
#1642=VECTOR('',#12689,10.);
#1643=VECTOR('',#12690,10.);
#1644=VECTOR('',#12691,10.);
#1645=VECTOR('',#12694,10.);
#1646=VECTOR('',#12697,10.);
#1647=VECTOR('',#12700,10.);
#1648=VECTOR('',#12703,10.);
#1649=VECTOR('',#12704,10.);
#1650=VECTOR('',#12705,10.);
#1651=VECTOR('',#12708,10.);
#1652=VECTOR('',#12713,10.);
#1653=VECTOR('',#12718,10.);
#1654=VECTOR('',#12723,10.);
#1655=VECTOR('',#12726,10.);
#1656=VECTOR('',#12731,10.);
#1657=VECTOR('',#12732,10.);
#1658=VECTOR('',#12735,10.);
#1659=VECTOR('',#12742,5.);
#1660=VECTOR('',#12743,10.);
#1661=VECTOR('',#12746,10.);
#1662=VECTOR('',#12751,5.);
#1663=VECTOR('',#12758,5.);
#1664=VECTOR('',#12765,5.);
#1665=VECTOR('',#12768,10.);
#1666=VECTOR('',#12769,10.);
#1667=VECTOR('',#12776,12.5);
#1668=VECTOR('',#12783,5.);
#1669=VECTOR('',#12786,10.);
#1670=VECTOR('',#12787,10.);
#1671=VECTOR('',#12794,5.);
#1672=VECTOR('',#12801,5.);
#1673=VECTOR('',#12804,10.);
#1674=VECTOR('',#12805,10.);
#1675=VECTOR('',#12812,5.);
#1676=VECTOR('',#12819,5.);
#1677=VECTOR('',#12820,10.);
#1678=VECTOR('',#12823,10.);
#1679=VECTOR('',#12828,5.);
#1680=VECTOR('',#12835,5.);
#1681=VECTOR('',#12838,10.);
#1682=VECTOR('',#12839,10.);
#1683=VECTOR('',#12846,5.);
#1684=VECTOR('',#12849,10.);
#1685=VECTOR('',#12852,10.);
#1686=VECTOR('',#12867,12.5);
#1687=VECTOR('',#12870,10.);
#1688=VECTOR('',#12871,10.);
#1689=VECTOR('',#12878,5.);
#1690=VECTOR('',#12881,10.);
#1691=VECTOR('',#12884,10.);
#1692=VECTOR('',#12899,5.);
#1693=VECTOR('',#12902,10.);
#1694=VECTOR('',#12905,10.);
#1695=VECTOR('',#12920,5.);
#1696=VECTOR('',#12923,10.);
#1697=VECTOR('',#12926,10.);
#1698=VECTOR('',#12941,5.);
#1699=VECTOR('',#12948,5.);
#1700=VECTOR('',#12949,10.);
#1701=VECTOR('',#12952,10.);
#1702=VECTOR('',#12955,10.);
#1703=VECTOR('',#12960,10.);
#1704=VECTOR('',#12963,10.);
#1705=VECTOR('',#12966,10.);
#1706=VECTOR('',#12971,10.);
#1707=VECTOR('',#12974,10.);
#1708=VECTOR('',#12975,10.);
#1709=VECTOR('',#12978,10.);
#1710=VECTOR('',#12981,10.);
#1711=VECTOR('',#12982,10.);
#1712=VECTOR('',#12985,10.);
#1713=VECTOR('',#12988,10.);
#1714=VECTOR('',#12993,10.);
#1715=VECTOR('',#12996,10.);
#1716=VECTOR('',#12999,10.);
#1717=VECTOR('',#13004,10.);
#1718=VECTOR('',#13007,10.);
#1719=VECTOR('',#13010,10.);
#1720=VECTOR('',#13011,10.);
#1721=VECTOR('',#13014,10.);
#1722=VECTOR('',#13017,10.);
#1723=VECTOR('',#13020,10.);
#1724=VECTOR('',#13021,10.);
#1725=VECTOR('',#13024,10.);
#1726=VECTOR('',#13025,10.);
#1727=VECTOR('',#13028,10.);
#1728=VECTOR('',#13029,10.);
#1729=VECTOR('',#13032,10.);
#1730=VECTOR('',#13035,10.);
#1731=VECTOR('',#13036,10.);
#1732=VECTOR('',#13039,10.);
#1733=VECTOR('',#13042,10.);
#1734=VECTOR('',#13045,10.);
#1735=VECTOR('',#13048,10.);
#1736=VECTOR('',#13051,10.);
#1737=VECTOR('',#13052,10.);
#1738=VECTOR('',#13055,10.);
#1739=VECTOR('',#13058,10.);
#1740=VECTOR('',#13061,10.);
#1741=VECTOR('',#13062,10.);
#1742=VECTOR('',#13067,10.);
#1743=VECTOR('',#13070,10.);
#1744=VECTOR('',#13073,10.);
#1745=VECTOR('',#13078,10.);
#1746=VECTOR('',#13081,10.);
#1747=VECTOR('',#13084,10.);
#1748=VECTOR('',#13085,10.);
#1749=VECTOR('',#13088,10.);
#1750=VECTOR('',#13091,10.);
#1751=VECTOR('',#13092,10.);
#1752=VECTOR('',#13095,10.);
#1753=VECTOR('',#13098,10.);
#1754=VECTOR('',#13099,10.);
#1755=VECTOR('',#13102,10.);
#1756=VECTOR('',#13103,10.);
#1757=VECTOR('',#13106,10.);
#1758=VECTOR('',#13109,10.);
#1759=VECTOR('',#13124,10.);
#1760=VECTOR('',#13125,10.);
#1761=VECTOR('',#13126,10.);
#1762=VECTOR('',#13127,10.);
#1763=VECTOR('',#13128,10.);
#1764=VECTOR('',#13129,10.);
#1765=VECTOR('',#13130,10.);
#1766=VECTOR('',#13131,10.);
#1767=VECTOR('',#13134,10.);
#1768=VECTOR('',#13137,10.);
#1769=VECTOR('',#13142,10.);
#1770=VECTOR('',#13145,10.);
#1771=VECTOR('',#13148,10.);
#1772=VECTOR('',#13151,10.);
#1773=VECTOR('',#13152,10.);
#1774=VECTOR('',#13155,10.);
#1775=VECTOR('',#13158,10.);
#1776=VECTOR('',#13161,10.);
#1777=VECTOR('',#13174,10.);
#1778=VECTOR('',#13175,10.);
#1779=VECTOR('',#13176,10.);
#1780=VECTOR('',#13179,10.);
#1781=VECTOR('',#13180,10.);
#1782=VECTOR('',#13181,10.);
#1783=VECTOR('',#13182,10.);
#1784=VECTOR('',#13205,10.);
#1785=VECTOR('',#13232,10.);
#1786=VECTOR('',#13241,10.);
#1787=VECTOR('',#13252,10.);
#1788=VECTOR('',#13269,10.);
#1789=VECTOR('',#13278,10.);
#1790=VECTOR('',#13289,10.);
#1791=VECTOR('',#13290,10.);
#1792=VECTOR('',#13307,10.);
#1793=VECTOR('',#13308,10.);
#1794=VECTOR('',#13319,10.);
#1795=VECTOR('',#13352,10.);
#1796=VECTOR('',#13385,10.);
#1797=VECTOR('',#13388,10.);
#1798=VECTOR('',#13399,10.);
#1799=VECTOR('',#13402,10.);
#1800=VECTOR('',#13405,10.);
#1801=VECTOR('',#13408,10.);
#1802=VECTOR('',#13409,10.);
#1803=VECTOR('',#13412,10.);
#1804=VECTOR('',#13415,10.);
#1805=VECTOR('',#13418,10.);
#1806=VECTOR('',#13419,10.);
#1807=VECTOR('',#13422,10.);
#1808=VECTOR('',#13423,10.);
#1809=VECTOR('',#13426,10.);
#1810=VECTOR('',#13427,10.);
#1811=VECTOR('',#13430,10.);
#1812=VECTOR('',#13433,10.);
#1813=VECTOR('',#13434,10.);
#1814=VECTOR('',#13437,10.);
#1815=VECTOR('',#13438,10.);
#1816=VECTOR('',#13441,10.);
#1817=VECTOR('',#13444,10.);
#1818=VECTOR('',#13447,10.);
#1819=VECTOR('',#13450,10.);
#1820=VECTOR('',#13453,10.);
#1821=VECTOR('',#13456,10.);
#1822=VECTOR('',#13459,10.);
#1823=VECTOR('',#13462,10.);
#1824=VECTOR('',#13463,10.);
#1825=VECTOR('',#13488,10.);
#1826=VECTOR('',#13491,10.);
#1827=VECTOR('',#13504,10.);
#1828=VECTOR('',#13505,10.);
#1829=VECTOR('',#13514,10.);
#1830=VECTOR('',#13517,10.);
#1831=VECTOR('',#13520,10.);
#1832=VECTOR('',#13521,10.);
#1833=VECTOR('',#13524,10.);
#1834=VECTOR('',#13525,10.);
#1835=VECTOR('',#13526,10.);
#1836=VECTOR('',#13527,10.);
#1837=VECTOR('',#13558,10.);
#1838=VECTOR('',#13559,10.);
#1839=VECTOR('',#13580,10.);
#1840=VECTOR('',#13581,10.);
#1841=VECTOR('',#13616,10.);
#1842=VECTOR('',#13617,10.);
#1843=VECTOR('',#13628,10.);
#1844=VECTOR('',#13629,10.);
#1845=VECTOR('',#13632,10.);
#1846=VECTOR('',#13633,10.);
#1847=VECTOR('',#13636,10.);
#1848=VECTOR('',#13637,10.);
#1849=VECTOR('',#13640,10.);
#1850=VECTOR('',#13641,10.);
#1851=VECTOR('',#13644,10.);
#1852=VECTOR('',#13645,10.);
#1853=VECTOR('',#13648,10.);
#1854=VECTOR('',#13649,10.);
#1855=VECTOR('',#13652,10.);
#1856=VECTOR('',#13655,10.);
#1857=VECTOR('',#13658,10.);
#1858=VECTOR('',#13659,10.);
#1859=VECTOR('',#13662,10.);
#1860=VECTOR('',#13663,10.);
#1861=VECTOR('',#13666,10.);
#1862=VECTOR('',#13669,10.);
#1863=VECTOR('',#13672,10.);
#1864=VECTOR('',#13673,10.);
#1865=VECTOR('',#13678,10.);
#1866=VECTOR('',#13679,10.);
#1867=VECTOR('',#13682,10.);
#1868=VECTOR('',#13689,10.);
#1869=VECTOR('',#13692,10.);
#1870=VECTOR('',#13715,10.);
#1871=VECTOR('',#13720,10.);
#1872=VECTOR('',#13737,8.5);
#1873=VECTOR('',#13742,9.);
#1874=VECTOR('',#13749,8.5);
#1875=VECTOR('',#13752,7.5);
#1876=VECTOR('',#13763,10.);
#1877=VECTOR('',#13766,10.);
#1878=VECTOR('',#13779,10.);
#1879=VECTOR('',#13780,10.);
#1880=VECTOR('',#13789,10.);
#1881=VECTOR('',#13792,10.);
#1882=VECTOR('',#13795,10.);
#1883=VECTOR('',#13796,10.);
#1884=VECTOR('',#13799,10.);
#1885=VECTOR('',#13800,10.);
#1886=VECTOR('',#13801,10.);
#1887=VECTOR('',#13802,10.);
#1888=VECTOR('',#13833,10.);
#1889=VECTOR('',#13836,10.);
#1890=VECTOR('',#13855,10.);
#1891=VECTOR('',#13856,10.);
#1892=VECTOR('',#13891,10.);
#1893=VECTOR('',#13892,10.);
#1894=VECTOR('',#13903,10.);
#1895=VECTOR('',#13904,10.);
#1896=VECTOR('',#13907,10.);
#1897=VECTOR('',#13908,10.);
#1898=VECTOR('',#13911,10.);
#1899=VECTOR('',#13912,10.);
#1900=VECTOR('',#13915,10.);
#1901=VECTOR('',#13916,10.);
#1902=VECTOR('',#13919,10.);
#1903=VECTOR('',#13920,10.);
#1904=VECTOR('',#13923,10.);
#1905=VECTOR('',#13924,10.);
#1906=VECTOR('',#13927,10.);
#1907=VECTOR('',#13930,10.);
#1908=VECTOR('',#13933,10.);
#1909=VECTOR('',#13934,10.);
#1910=VECTOR('',#13937,10.);
#1911=VECTOR('',#13938,10.);
#1912=VECTOR('',#13941,10.);
#1913=VECTOR('',#13944,10.);
#1914=VECTOR('',#13947,10.);
#1915=VECTOR('',#13950,10.);
#1916=VECTOR('',#13953,10.);
#1917=VECTOR('',#13954,10.);
#1918=VECTOR('',#13957,10.);
#1919=VECTOR('',#13964,10.);
#1920=VECTOR('',#13967,10.);
#1921=VECTOR('',#13990,10.);
#1922=VECTOR('',#13995,10.);
#1923=VECTOR('',#14006,10.);
#1924=VECTOR('',#14009,10.);
#1925=VECTOR('',#14022,10.);
#1926=VECTOR('',#14023,10.);
#1927=VECTOR('',#14032,10.);
#1928=VECTOR('',#14035,10.);
#1929=VECTOR('',#14038,10.);
#1930=VECTOR('',#14039,10.);
#1931=VECTOR('',#14042,10.);
#1932=VECTOR('',#14043,10.);
#1933=VECTOR('',#14044,10.);
#1934=VECTOR('',#14045,10.);
#1935=VECTOR('',#14076,10.);
#1936=VECTOR('',#14077,10.);
#1937=VECTOR('',#14098,10.);
#1938=VECTOR('',#14099,10.);
#1939=VECTOR('',#14134,10.);
#1940=VECTOR('',#14135,10.);
#1941=VECTOR('',#14146,10.);
#1942=VECTOR('',#14147,10.);
#1943=VECTOR('',#14150,10.);
#1944=VECTOR('',#14151,10.);
#1945=VECTOR('',#14154,10.);
#1946=VECTOR('',#14155,10.);
#1947=VECTOR('',#14158,10.);
#1948=VECTOR('',#14159,10.);
#1949=VECTOR('',#14162,10.);
#1950=VECTOR('',#14163,10.);
#1951=VECTOR('',#14166,10.);
#1952=VECTOR('',#14167,10.);
#1953=VECTOR('',#14170,10.);
#1954=VECTOR('',#14173,10.);
#1955=VECTOR('',#14176,10.);
#1956=VECTOR('',#14177,10.);
#1957=VECTOR('',#14180,10.);
#1958=VECTOR('',#14181,10.);
#1959=VECTOR('',#14184,10.);
#1960=VECTOR('',#14187,10.);
#1961=VECTOR('',#14190,10.);
#1962=VECTOR('',#14191,10.);
#1963=VECTOR('',#14196,10.);
#1964=VECTOR('',#14197,10.);
#1965=VECTOR('',#14200,10.);
#1966=VECTOR('',#14207,10.);
#1967=VECTOR('',#14210,10.);
#1968=VECTOR('',#14233,10.);
#1969=VECTOR('',#14238,10.);
#1970=CONICAL_SURFACE('',#9754,8.5,0.78539816339745);
#1971=CONICAL_SURFACE('',#9760,8.5,0.78539816339745);
#1972=CONICAL_SURFACE('',#10816,8.5,0.78539816339745);
#1973=CONICAL_SURFACE('',#10822,8.5,0.78539816339745);
#1974=FACE_BOUND('',#2642,.T.);
#1975=FACE_BOUND('',#2801,.T.);
#1976=FACE_BOUND('',#2802,.T.);
#1977=FACE_BOUND('',#2809,.T.);
#1978=FACE_BOUND('',#2810,.T.);
#1979=FACE_BOUND('',#2811,.T.);
#1980=FACE_BOUND('',#2812,.T.);
#1981=FACE_BOUND('',#2841,.T.);
#1982=FACE_BOUND('',#2842,.T.);
#1983=FACE_BOUND('',#2843,.T.);
#1984=FACE_BOUND('',#2844,.T.);
#1985=FACE_BOUND('',#2854,.T.);
#1986=FACE_BOUND('',#2855,.T.);
#1987=FACE_BOUND('',#2856,.T.);
#1988=FACE_BOUND('',#2857,.T.);
#1989=FACE_BOUND('',#2932,.T.);
#1990=FACE_BOUND('',#2964,.T.);
#1991=FACE_BOUND('',#3058,.T.);
#1992=FACE_BOUND('',#3059,.T.);
#1993=FACE_BOUND('',#3060,.T.);
#1994=FACE_BOUND('',#3062,.T.);
#1995=FACE_BOUND('',#3063,.T.);
#1996=FACE_BOUND('',#3064,.T.);
#1997=FACE_BOUND('',#3065,.T.);
#1998=FACE_BOUND('',#3066,.T.);
#1999=FACE_BOUND('',#3129,.T.);
#2000=FACE_BOUND('',#3130,.T.);
#2001=FACE_BOUND('',#3131,.T.);
#2002=FACE_BOUND('',#3132,.T.);
#2003=FACE_BOUND('',#3133,.T.);
#2004=FACE_BOUND('',#3134,.T.);
#2005=FACE_BOUND('',#3135,.T.);
#2006=FACE_BOUND('',#3136,.T.);
#2007=FACE_BOUND('',#3137,.T.);
#2008=FACE_BOUND('',#3138,.T.);
#2009=FACE_BOUND('',#3139,.T.);
#2010=FACE_BOUND('',#3140,.T.);
#2011=FACE_BOUND('',#3141,.T.);
#2012=FACE_BOUND('',#3142,.T.);
#2013=FACE_BOUND('',#3143,.T.);
#2014=FACE_BOUND('',#3144,.T.);
#2015=FACE_BOUND('',#3145,.T.);
#2016=FACE_BOUND('',#3146,.T.);
#2017=FACE_BOUND('',#3147,.T.);
#2018=FACE_BOUND('',#3148,.T.);
#2019=FACE_BOUND('',#3149,.T.);
#2020=FACE_BOUND('',#3160,.T.);
#2021=FACE_BOUND('',#3192,.T.);
#2022=FACE_BOUND('',#3203,.T.);
#2023=FACE_BOUND('',#3217,.T.);
#2024=FACE_BOUND('',#3249,.T.);
#2025=FACE_BOUND('',#3266,.T.);
#2026=FACE_BOUND('',#3298,.T.);
#2027=FACE_OUTER_BOUND('',#2641,.T.);
#2028=FACE_OUTER_BOUND('',#2643,.T.);
#2029=FACE_OUTER_BOUND('',#2644,.T.);
#2030=FACE_OUTER_BOUND('',#2645,.T.);
#2031=FACE_OUTER_BOUND('',#2646,.T.);
#2032=FACE_OUTER_BOUND('',#2647,.T.);
#2033=FACE_OUTER_BOUND('',#2648,.T.);
#2034=FACE_OUTER_BOUND('',#2649,.T.);
#2035=FACE_OUTER_BOUND('',#2650,.T.);
#2036=FACE_OUTER_BOUND('',#2651,.T.);
#2037=FACE_OUTER_BOUND('',#2652,.T.);
#2038=FACE_OUTER_BOUND('',#2653,.T.);
#2039=FACE_OUTER_BOUND('',#2654,.T.);
#2040=FACE_OUTER_BOUND('',#2655,.T.);
#2041=FACE_OUTER_BOUND('',#2656,.T.);
#2042=FACE_OUTER_BOUND('',#2657,.T.);
#2043=FACE_OUTER_BOUND('',#2658,.T.);
#2044=FACE_OUTER_BOUND('',#2659,.T.);
#2045=FACE_OUTER_BOUND('',#2660,.T.);
#2046=FACE_OUTER_BOUND('',#2661,.T.);
#2047=FACE_OUTER_BOUND('',#2662,.T.);
#2048=FACE_OUTER_BOUND('',#2663,.T.);
#2049=FACE_OUTER_BOUND('',#2664,.T.);
#2050=FACE_OUTER_BOUND('',#2665,.T.);
#2051=FACE_OUTER_BOUND('',#2666,.T.);
#2052=FACE_OUTER_BOUND('',#2667,.T.);
#2053=FACE_OUTER_BOUND('',#2668,.T.);
#2054=FACE_OUTER_BOUND('',#2669,.T.);
#2055=FACE_OUTER_BOUND('',#2670,.T.);
#2056=FACE_OUTER_BOUND('',#2671,.T.);
#2057=FACE_OUTER_BOUND('',#2672,.T.);
#2058=FACE_OUTER_BOUND('',#2673,.T.);
#2059=FACE_OUTER_BOUND('',#2674,.T.);
#2060=FACE_OUTER_BOUND('',#2675,.T.);
#2061=FACE_OUTER_BOUND('',#2676,.T.);
#2062=FACE_OUTER_BOUND('',#2677,.T.);
#2063=FACE_OUTER_BOUND('',#2678,.T.);
#2064=FACE_OUTER_BOUND('',#2679,.T.);
#2065=FACE_OUTER_BOUND('',#2680,.T.);
#2066=FACE_OUTER_BOUND('',#2681,.T.);
#2067=FACE_OUTER_BOUND('',#2682,.T.);
#2068=FACE_OUTER_BOUND('',#2683,.T.);
#2069=FACE_OUTER_BOUND('',#2684,.T.);
#2070=FACE_OUTER_BOUND('',#2685,.T.);
#2071=FACE_OUTER_BOUND('',#2686,.T.);
#2072=FACE_OUTER_BOUND('',#2687,.T.);
#2073=FACE_OUTER_BOUND('',#2688,.T.);
#2074=FACE_OUTER_BOUND('',#2689,.T.);
#2075=FACE_OUTER_BOUND('',#2690,.T.);
#2076=FACE_OUTER_BOUND('',#2691,.T.);
#2077=FACE_OUTER_BOUND('',#2692,.T.);
#2078=FACE_OUTER_BOUND('',#2693,.T.);
#2079=FACE_OUTER_BOUND('',#2694,.T.);
#2080=FACE_OUTER_BOUND('',#2695,.T.);
#2081=FACE_OUTER_BOUND('',#2696,.T.);
#2082=FACE_OUTER_BOUND('',#2697,.T.);
#2083=FACE_OUTER_BOUND('',#2698,.T.);
#2084=FACE_OUTER_BOUND('',#2699,.T.);
#2085=FACE_OUTER_BOUND('',#2700,.T.);
#2086=FACE_OUTER_BOUND('',#2701,.T.);
#2087=FACE_OUTER_BOUND('',#2702,.T.);
#2088=FACE_OUTER_BOUND('',#2703,.T.);
#2089=FACE_OUTER_BOUND('',#2704,.T.);
#2090=FACE_OUTER_BOUND('',#2705,.T.);
#2091=FACE_OUTER_BOUND('',#2706,.T.);
#2092=FACE_OUTER_BOUND('',#2707,.T.);
#2093=FACE_OUTER_BOUND('',#2708,.T.);
#2094=FACE_OUTER_BOUND('',#2709,.T.);
#2095=FACE_OUTER_BOUND('',#2710,.T.);
#2096=FACE_OUTER_BOUND('',#2711,.T.);
#2097=FACE_OUTER_BOUND('',#2712,.T.);
#2098=FACE_OUTER_BOUND('',#2713,.T.);
#2099=FACE_OUTER_BOUND('',#2714,.T.);
#2100=FACE_OUTER_BOUND('',#2715,.T.);
#2101=FACE_OUTER_BOUND('',#2716,.T.);
#2102=FACE_OUTER_BOUND('',#2717,.T.);
#2103=FACE_OUTER_BOUND('',#2718,.T.);
#2104=FACE_OUTER_BOUND('',#2719,.T.);
#2105=FACE_OUTER_BOUND('',#2720,.T.);
#2106=FACE_OUTER_BOUND('',#2721,.T.);
#2107=FACE_OUTER_BOUND('',#2722,.T.);
#2108=FACE_OUTER_BOUND('',#2723,.T.);
#2109=FACE_OUTER_BOUND('',#2724,.T.);
#2110=FACE_OUTER_BOUND('',#2725,.T.);
#2111=FACE_OUTER_BOUND('',#2726,.T.);
#2112=FACE_OUTER_BOUND('',#2727,.T.);
#2113=FACE_OUTER_BOUND('',#2728,.T.);
#2114=FACE_OUTER_BOUND('',#2729,.T.);
#2115=FACE_OUTER_BOUND('',#2730,.T.);
#2116=FACE_OUTER_BOUND('',#2731,.T.);
#2117=FACE_OUTER_BOUND('',#2732,.T.);
#2118=FACE_OUTER_BOUND('',#2733,.T.);
#2119=FACE_OUTER_BOUND('',#2734,.T.);
#2120=FACE_OUTER_BOUND('',#2735,.T.);
#2121=FACE_OUTER_BOUND('',#2736,.T.);
#2122=FACE_OUTER_BOUND('',#2737,.T.);
#2123=FACE_OUTER_BOUND('',#2738,.T.);
#2124=FACE_OUTER_BOUND('',#2739,.T.);
#2125=FACE_OUTER_BOUND('',#2740,.T.);
#2126=FACE_OUTER_BOUND('',#2741,.T.);
#2127=FACE_OUTER_BOUND('',#2742,.T.);
#2128=FACE_OUTER_BOUND('',#2743,.T.);
#2129=FACE_OUTER_BOUND('',#2744,.T.);
#2130=FACE_OUTER_BOUND('',#2745,.T.);
#2131=FACE_OUTER_BOUND('',#2746,.T.);
#2132=FACE_OUTER_BOUND('',#2747,.T.);
#2133=FACE_OUTER_BOUND('',#2748,.T.);
#2134=FACE_OUTER_BOUND('',#2749,.T.);
#2135=FACE_OUTER_BOUND('',#2750,.T.);
#2136=FACE_OUTER_BOUND('',#2751,.T.);
#2137=FACE_OUTER_BOUND('',#2752,.T.);
#2138=FACE_OUTER_BOUND('',#2753,.T.);
#2139=FACE_OUTER_BOUND('',#2754,.T.);
#2140=FACE_OUTER_BOUND('',#2755,.T.);
#2141=FACE_OUTER_BOUND('',#2756,.T.);
#2142=FACE_OUTER_BOUND('',#2757,.T.);
#2143=FACE_OUTER_BOUND('',#2758,.T.);
#2144=FACE_OUTER_BOUND('',#2759,.T.);
#2145=FACE_OUTER_BOUND('',#2760,.T.);
#2146=FACE_OUTER_BOUND('',#2761,.T.);
#2147=FACE_OUTER_BOUND('',#2762,.T.);
#2148=FACE_OUTER_BOUND('',#2763,.T.);
#2149=FACE_OUTER_BOUND('',#2764,.T.);
#2150=FACE_OUTER_BOUND('',#2765,.T.);
#2151=FACE_OUTER_BOUND('',#2766,.T.);
#2152=FACE_OUTER_BOUND('',#2767,.T.);
#2153=FACE_OUTER_BOUND('',#2768,.T.);
#2154=FACE_OUTER_BOUND('',#2769,.T.);
#2155=FACE_OUTER_BOUND('',#2770,.T.);
#2156=FACE_OUTER_BOUND('',#2771,.T.);
#2157=FACE_OUTER_BOUND('',#2772,.T.);
#2158=FACE_OUTER_BOUND('',#2773,.T.);
#2159=FACE_OUTER_BOUND('',#2774,.T.);
#2160=FACE_OUTER_BOUND('',#2775,.T.);
#2161=FACE_OUTER_BOUND('',#2776,.T.);
#2162=FACE_OUTER_BOUND('',#2777,.T.);
#2163=FACE_OUTER_BOUND('',#2778,.T.);
#2164=FACE_OUTER_BOUND('',#2779,.T.);
#2165=FACE_OUTER_BOUND('',#2780,.T.);
#2166=FACE_OUTER_BOUND('',#2781,.T.);
#2167=FACE_OUTER_BOUND('',#2782,.T.);
#2168=FACE_OUTER_BOUND('',#2783,.T.);
#2169=FACE_OUTER_BOUND('',#2784,.T.);
#2170=FACE_OUTER_BOUND('',#2785,.T.);
#2171=FACE_OUTER_BOUND('',#2786,.T.);
#2172=FACE_OUTER_BOUND('',#2787,.T.);
#2173=FACE_OUTER_BOUND('',#2788,.T.);
#2174=FACE_OUTER_BOUND('',#2789,.T.);
#2175=FACE_OUTER_BOUND('',#2790,.T.);
#2176=FACE_OUTER_BOUND('',#2791,.T.);
#2177=FACE_OUTER_BOUND('',#2792,.T.);
#2178=FACE_OUTER_BOUND('',#2793,.T.);
#2179=FACE_OUTER_BOUND('',#2794,.T.);
#2180=FACE_OUTER_BOUND('',#2795,.T.);
#2181=FACE_OUTER_BOUND('',#2796,.T.);
#2182=FACE_OUTER_BOUND('',#2797,.T.);
#2183=FACE_OUTER_BOUND('',#2798,.T.);
#2184=FACE_OUTER_BOUND('',#2799,.T.);
#2185=FACE_OUTER_BOUND('',#2800,.T.);
#2186=FACE_OUTER_BOUND('',#2803,.T.);
#2187=FACE_OUTER_BOUND('',#2804,.T.);
#2188=FACE_OUTER_BOUND('',#2805,.T.);
#2189=FACE_OUTER_BOUND('',#2806,.T.);
#2190=FACE_OUTER_BOUND('',#2807,.T.);
#2191=FACE_OUTER_BOUND('',#2808,.T.);
#2192=FACE_OUTER_BOUND('',#2813,.T.);
#2193=FACE_OUTER_BOUND('',#2814,.T.);
#2194=FACE_OUTER_BOUND('',#2815,.T.);
#2195=FACE_OUTER_BOUND('',#2816,.T.);
#2196=FACE_OUTER_BOUND('',#2817,.T.);
#2197=FACE_OUTER_BOUND('',#2818,.T.);
#2198=FACE_OUTER_BOUND('',#2819,.T.);
#2199=FACE_OUTER_BOUND('',#2820,.T.);
#2200=FACE_OUTER_BOUND('',#2821,.T.);
#2201=FACE_OUTER_BOUND('',#2822,.T.);
#2202=FACE_OUTER_BOUND('',#2823,.T.);
#2203=FACE_OUTER_BOUND('',#2824,.T.);
#2204=FACE_OUTER_BOUND('',#2825,.T.);
#2205=FACE_OUTER_BOUND('',#2826,.T.);
#2206=FACE_OUTER_BOUND('',#2827,.T.);
#2207=FACE_OUTER_BOUND('',#2828,.T.);
#2208=FACE_OUTER_BOUND('',#2829,.T.);
#2209=FACE_OUTER_BOUND('',#2830,.T.);
#2210=FACE_OUTER_BOUND('',#2831,.T.);
#2211=FACE_OUTER_BOUND('',#2832,.T.);
#2212=FACE_OUTER_BOUND('',#2833,.T.);
#2213=FACE_OUTER_BOUND('',#2834,.T.);
#2214=FACE_OUTER_BOUND('',#2835,.T.);
#2215=FACE_OUTER_BOUND('',#2836,.T.);
#2216=FACE_OUTER_BOUND('',#2837,.T.);
#2217=FACE_OUTER_BOUND('',#2838,.T.);
#2218=FACE_OUTER_BOUND('',#2839,.T.);
#2219=FACE_OUTER_BOUND('',#2840,.T.);
#2220=FACE_OUTER_BOUND('',#2845,.T.);
#2221=FACE_OUTER_BOUND('',#2846,.T.);
#2222=FACE_OUTER_BOUND('',#2847,.T.);
#2223=FACE_OUTER_BOUND('',#2848,.T.);
#2224=FACE_OUTER_BOUND('',#2849,.T.);
#2225=FACE_OUTER_BOUND('',#2850,.T.);
#2226=FACE_OUTER_BOUND('',#2851,.T.);
#2227=FACE_OUTER_BOUND('',#2852,.T.);
#2228=FACE_OUTER_BOUND('',#2853,.T.);
#2229=FACE_OUTER_BOUND('',#2858,.T.);
#2230=FACE_OUTER_BOUND('',#2859,.T.);
#2231=FACE_OUTER_BOUND('',#2860,.T.);
#2232=FACE_OUTER_BOUND('',#2861,.T.);
#2233=FACE_OUTER_BOUND('',#2862,.T.);
#2234=FACE_OUTER_BOUND('',#2863,.T.);
#2235=FACE_OUTER_BOUND('',#2864,.T.);
#2236=FACE_OUTER_BOUND('',#2865,.T.);
#2237=FACE_OUTER_BOUND('',#2866,.T.);
#2238=FACE_OUTER_BOUND('',#2867,.T.);
#2239=FACE_OUTER_BOUND('',#2868,.T.);
#2240=FACE_OUTER_BOUND('',#2869,.T.);
#2241=FACE_OUTER_BOUND('',#2870,.T.);
#2242=FACE_OUTER_BOUND('',#2871,.T.);
#2243=FACE_OUTER_BOUND('',#2872,.T.);
#2244=FACE_OUTER_BOUND('',#2873,.T.);
#2245=FACE_OUTER_BOUND('',#2874,.T.);
#2246=FACE_OUTER_BOUND('',#2875,.T.);
#2247=FACE_OUTER_BOUND('',#2876,.T.);
#2248=FACE_OUTER_BOUND('',#2877,.T.);
#2249=FACE_OUTER_BOUND('',#2878,.T.);
#2250=FACE_OUTER_BOUND('',#2879,.T.);
#2251=FACE_OUTER_BOUND('',#2880,.T.);
#2252=FACE_OUTER_BOUND('',#2881,.T.);
#2253=FACE_OUTER_BOUND('',#2882,.T.);
#2254=FACE_OUTER_BOUND('',#2883,.T.);
#2255=FACE_OUTER_BOUND('',#2884,.T.);
#2256=FACE_OUTER_BOUND('',#2885,.T.);
#2257=FACE_OUTER_BOUND('',#2886,.T.);
#2258=FACE_OUTER_BOUND('',#2887,.T.);
#2259=FACE_OUTER_BOUND('',#2888,.T.);
#2260=FACE_OUTER_BOUND('',#2889,.T.);
#2261=FACE_OUTER_BOUND('',#2890,.T.);
#2262=FACE_OUTER_BOUND('',#2891,.T.);
#2263=FACE_OUTER_BOUND('',#2892,.T.);
#2264=FACE_OUTER_BOUND('',#2893,.T.);
#2265=FACE_OUTER_BOUND('',#2894,.T.);
#2266=FACE_OUTER_BOUND('',#2895,.T.);
#2267=FACE_OUTER_BOUND('',#2896,.T.);
#2268=FACE_OUTER_BOUND('',#2897,.T.);
#2269=FACE_OUTER_BOUND('',#2898,.T.);
#2270=FACE_OUTER_BOUND('',#2899,.T.);
#2271=FACE_OUTER_BOUND('',#2900,.T.);
#2272=FACE_OUTER_BOUND('',#2901,.T.);
#2273=FACE_OUTER_BOUND('',#2902,.T.);
#2274=FACE_OUTER_BOUND('',#2903,.T.);
#2275=FACE_OUTER_BOUND('',#2904,.T.);
#2276=FACE_OUTER_BOUND('',#2905,.T.);
#2277=FACE_OUTER_BOUND('',#2906,.T.);
#2278=FACE_OUTER_BOUND('',#2907,.T.);
#2279=FACE_OUTER_BOUND('',#2908,.T.);
#2280=FACE_OUTER_BOUND('',#2909,.T.);
#2281=FACE_OUTER_BOUND('',#2910,.T.);
#2282=FACE_OUTER_BOUND('',#2911,.T.);
#2283=FACE_OUTER_BOUND('',#2912,.T.);
#2284=FACE_OUTER_BOUND('',#2913,.T.);
#2285=FACE_OUTER_BOUND('',#2914,.T.);
#2286=FACE_OUTER_BOUND('',#2915,.T.);
#2287=FACE_OUTER_BOUND('',#2916,.T.);
#2288=FACE_OUTER_BOUND('',#2917,.T.);
#2289=FACE_OUTER_BOUND('',#2918,.T.);
#2290=FACE_OUTER_BOUND('',#2919,.T.);
#2291=FACE_OUTER_BOUND('',#2920,.T.);
#2292=FACE_OUTER_BOUND('',#2921,.T.);
#2293=FACE_OUTER_BOUND('',#2922,.T.);
#2294=FACE_OUTER_BOUND('',#2923,.T.);
#2295=FACE_OUTER_BOUND('',#2924,.T.);
#2296=FACE_OUTER_BOUND('',#2925,.T.);
#2297=FACE_OUTER_BOUND('',#2926,.T.);
#2298=FACE_OUTER_BOUND('',#2927,.T.);
#2299=FACE_OUTER_BOUND('',#2928,.T.);
#2300=FACE_OUTER_BOUND('',#2929,.T.);
#2301=FACE_OUTER_BOUND('',#2930,.T.);
#2302=FACE_OUTER_BOUND('',#2931,.T.);
#2303=FACE_OUTER_BOUND('',#2933,.T.);
#2304=FACE_OUTER_BOUND('',#2934,.T.);
#2305=FACE_OUTER_BOUND('',#2935,.T.);
#2306=FACE_OUTER_BOUND('',#2936,.T.);
#2307=FACE_OUTER_BOUND('',#2937,.T.);
#2308=FACE_OUTER_BOUND('',#2938,.T.);
#2309=FACE_OUTER_BOUND('',#2939,.T.);
#2310=FACE_OUTER_BOUND('',#2940,.T.);
#2311=FACE_OUTER_BOUND('',#2941,.T.);
#2312=FACE_OUTER_BOUND('',#2942,.T.);
#2313=FACE_OUTER_BOUND('',#2943,.T.);
#2314=FACE_OUTER_BOUND('',#2944,.T.);
#2315=FACE_OUTER_BOUND('',#2945,.T.);
#2316=FACE_OUTER_BOUND('',#2946,.T.);
#2317=FACE_OUTER_BOUND('',#2947,.T.);
#2318=FACE_OUTER_BOUND('',#2948,.T.);
#2319=FACE_OUTER_BOUND('',#2949,.T.);
#2320=FACE_OUTER_BOUND('',#2950,.T.);
#2321=FACE_OUTER_BOUND('',#2951,.T.);
#2322=FACE_OUTER_BOUND('',#2952,.T.);
#2323=FACE_OUTER_BOUND('',#2953,.T.);
#2324=FACE_OUTER_BOUND('',#2954,.T.);
#2325=FACE_OUTER_BOUND('',#2955,.T.);
#2326=FACE_OUTER_BOUND('',#2956,.T.);
#2327=FACE_OUTER_BOUND('',#2957,.T.);
#2328=FACE_OUTER_BOUND('',#2958,.T.);
#2329=FACE_OUTER_BOUND('',#2959,.T.);
#2330=FACE_OUTER_BOUND('',#2960,.T.);
#2331=FACE_OUTER_BOUND('',#2961,.T.);
#2332=FACE_OUTER_BOUND('',#2962,.T.);
#2333=FACE_OUTER_BOUND('',#2963,.T.);
#2334=FACE_OUTER_BOUND('',#2965,.T.);
#2335=FACE_OUTER_BOUND('',#2966,.T.);
#2336=FACE_OUTER_BOUND('',#2967,.T.);
#2337=FACE_OUTER_BOUND('',#2968,.T.);
#2338=FACE_OUTER_BOUND('',#2969,.T.);
#2339=FACE_OUTER_BOUND('',#2970,.T.);
#2340=FACE_OUTER_BOUND('',#2971,.T.);
#2341=FACE_OUTER_BOUND('',#2972,.T.);
#2342=FACE_OUTER_BOUND('',#2973,.T.);
#2343=FACE_OUTER_BOUND('',#2974,.T.);
#2344=FACE_OUTER_BOUND('',#2975,.T.);
#2345=FACE_OUTER_BOUND('',#2976,.T.);
#2346=FACE_OUTER_BOUND('',#2977,.T.);
#2347=FACE_OUTER_BOUND('',#2978,.T.);
#2348=FACE_OUTER_BOUND('',#2979,.T.);
#2349=FACE_OUTER_BOUND('',#2980,.T.);
#2350=FACE_OUTER_BOUND('',#2981,.T.);
#2351=FACE_OUTER_BOUND('',#2982,.T.);
#2352=FACE_OUTER_BOUND('',#2983,.T.);
#2353=FACE_OUTER_BOUND('',#2984,.T.);
#2354=FACE_OUTER_BOUND('',#2985,.T.);
#2355=FACE_OUTER_BOUND('',#2986,.T.);
#2356=FACE_OUTER_BOUND('',#2987,.T.);
#2357=FACE_OUTER_BOUND('',#2988,.T.);
#2358=FACE_OUTER_BOUND('',#2989,.T.);
#2359=FACE_OUTER_BOUND('',#2990,.T.);
#2360=FACE_OUTER_BOUND('',#2991,.T.);
#2361=FACE_OUTER_BOUND('',#2992,.T.);
#2362=FACE_OUTER_BOUND('',#2993,.T.);
#2363=FACE_OUTER_BOUND('',#2994,.T.);
#2364=FACE_OUTER_BOUND('',#2995,.T.);
#2365=FACE_OUTER_BOUND('',#2996,.T.);
#2366=FACE_OUTER_BOUND('',#2997,.T.);
#2367=FACE_OUTER_BOUND('',#2998,.T.);
#2368=FACE_OUTER_BOUND('',#2999,.T.);
#2369=FACE_OUTER_BOUND('',#3000,.T.);
#2370=FACE_OUTER_BOUND('',#3001,.T.);
#2371=FACE_OUTER_BOUND('',#3002,.T.);
#2372=FACE_OUTER_BOUND('',#3003,.T.);
#2373=FACE_OUTER_BOUND('',#3004,.T.);
#2374=FACE_OUTER_BOUND('',#3005,.T.);
#2375=FACE_OUTER_BOUND('',#3006,.T.);
#2376=FACE_OUTER_BOUND('',#3007,.T.);
#2377=FACE_OUTER_BOUND('',#3008,.T.);
#2378=FACE_OUTER_BOUND('',#3009,.T.);
#2379=FACE_OUTER_BOUND('',#3010,.T.);
#2380=FACE_OUTER_BOUND('',#3011,.T.);
#2381=FACE_OUTER_BOUND('',#3012,.T.);
#2382=FACE_OUTER_BOUND('',#3013,.T.);
#2383=FACE_OUTER_BOUND('',#3014,.T.);
#2384=FACE_OUTER_BOUND('',#3015,.T.);
#2385=FACE_OUTER_BOUND('',#3016,.T.);
#2386=FACE_OUTER_BOUND('',#3017,.T.);
#2387=FACE_OUTER_BOUND('',#3018,.T.);
#2388=FACE_OUTER_BOUND('',#3019,.T.);
#2389=FACE_OUTER_BOUND('',#3020,.T.);
#2390=FACE_OUTER_BOUND('',#3021,.T.);
#2391=FACE_OUTER_BOUND('',#3022,.T.);
#2392=FACE_OUTER_BOUND('',#3023,.T.);
#2393=FACE_OUTER_BOUND('',#3024,.T.);
#2394=FACE_OUTER_BOUND('',#3025,.T.);
#2395=FACE_OUTER_BOUND('',#3026,.T.);
#2396=FACE_OUTER_BOUND('',#3027,.T.);
#2397=FACE_OUTER_BOUND('',#3028,.T.);
#2398=FACE_OUTER_BOUND('',#3029,.T.);
#2399=FACE_OUTER_BOUND('',#3030,.T.);
#2400=FACE_OUTER_BOUND('',#3031,.T.);
#2401=FACE_OUTER_BOUND('',#3032,.T.);
#2402=FACE_OUTER_BOUND('',#3033,.T.);
#2403=FACE_OUTER_BOUND('',#3034,.T.);
#2404=FACE_OUTER_BOUND('',#3035,.T.);
#2405=FACE_OUTER_BOUND('',#3036,.T.);
#2406=FACE_OUTER_BOUND('',#3037,.T.);
#2407=FACE_OUTER_BOUND('',#3038,.T.);
#2408=FACE_OUTER_BOUND('',#3039,.T.);
#2409=FACE_OUTER_BOUND('',#3040,.T.);
#2410=FACE_OUTER_BOUND('',#3041,.T.);
#2411=FACE_OUTER_BOUND('',#3042,.T.);
#2412=FACE_OUTER_BOUND('',#3043,.T.);
#2413=FACE_OUTER_BOUND('',#3044,.T.);
#2414=FACE_OUTER_BOUND('',#3045,.T.);
#2415=FACE_OUTER_BOUND('',#3046,.T.);
#2416=FACE_OUTER_BOUND('',#3047,.T.);
#2417=FACE_OUTER_BOUND('',#3048,.T.);
#2418=FACE_OUTER_BOUND('',#3049,.T.);
#2419=FACE_OUTER_BOUND('',#3050,.T.);
#2420=FACE_OUTER_BOUND('',#3051,.T.);
#2421=FACE_OUTER_BOUND('',#3052,.T.);
#2422=FACE_OUTER_BOUND('',#3053,.T.);
#2423=FACE_OUTER_BOUND('',#3054,.T.);
#2424=FACE_OUTER_BOUND('',#3055,.T.);
#2425=FACE_OUTER_BOUND('',#3056,.T.);
#2426=FACE_OUTER_BOUND('',#3057,.T.);
#2427=FACE_OUTER_BOUND('',#3061,.T.);
#2428=FACE_OUTER_BOUND('',#3067,.T.);
#2429=FACE_OUTER_BOUND('',#3068,.T.);
#2430=FACE_OUTER_BOUND('',#3069,.T.);
#2431=FACE_OUTER_BOUND('',#3070,.T.);
#2432=FACE_OUTER_BOUND('',#3071,.T.);
#2433=FACE_OUTER_BOUND('',#3072,.T.);
#2434=FACE_OUTER_BOUND('',#3073,.T.);
#2435=FACE_OUTER_BOUND('',#3074,.T.);
#2436=FACE_OUTER_BOUND('',#3075,.T.);
#2437=FACE_OUTER_BOUND('',#3076,.T.);
#2438=FACE_OUTER_BOUND('',#3077,.T.);
#2439=FACE_OUTER_BOUND('',#3078,.T.);
#2440=FACE_OUTER_BOUND('',#3079,.T.);
#2441=FACE_OUTER_BOUND('',#3080,.T.);
#2442=FACE_OUTER_BOUND('',#3081,.T.);
#2443=FACE_OUTER_BOUND('',#3082,.T.);
#2444=FACE_OUTER_BOUND('',#3083,.T.);
#2445=FACE_OUTER_BOUND('',#3084,.T.);
#2446=FACE_OUTER_BOUND('',#3085,.T.);
#2447=FACE_OUTER_BOUND('',#3086,.T.);
#2448=FACE_OUTER_BOUND('',#3087,.T.);
#2449=FACE_OUTER_BOUND('',#3088,.T.);
#2450=FACE_OUTER_BOUND('',#3089,.T.);
#2451=FACE_OUTER_BOUND('',#3090,.T.);
#2452=FACE_OUTER_BOUND('',#3091,.T.);
#2453=FACE_OUTER_BOUND('',#3092,.T.);
#2454=FACE_OUTER_BOUND('',#3093,.T.);
#2455=FACE_OUTER_BOUND('',#3094,.T.);
#2456=FACE_OUTER_BOUND('',#3095,.T.);
#2457=FACE_OUTER_BOUND('',#3096,.T.);
#2458=FACE_OUTER_BOUND('',#3097,.T.);
#2459=FACE_OUTER_BOUND('',#3098,.T.);
#2460=FACE_OUTER_BOUND('',#3099,.T.);
#2461=FACE_OUTER_BOUND('',#3100,.T.);
#2462=FACE_OUTER_BOUND('',#3101,.T.);
#2463=FACE_OUTER_BOUND('',#3102,.T.);
#2464=FACE_OUTER_BOUND('',#3103,.T.);
#2465=FACE_OUTER_BOUND('',#3104,.T.);
#2466=FACE_OUTER_BOUND('',#3105,.T.);
#2467=FACE_OUTER_BOUND('',#3106,.T.);
#2468=FACE_OUTER_BOUND('',#3107,.T.);
#2469=FACE_OUTER_BOUND('',#3108,.T.);
#2470=FACE_OUTER_BOUND('',#3109,.T.);
#2471=FACE_OUTER_BOUND('',#3110,.T.);
#2472=FACE_OUTER_BOUND('',#3111,.T.);
#2473=FACE_OUTER_BOUND('',#3112,.T.);
#2474=FACE_OUTER_BOUND('',#3113,.T.);
#2475=FACE_OUTER_BOUND('',#3114,.T.);
#2476=FACE_OUTER_BOUND('',#3115,.T.);
#2477=FACE_OUTER_BOUND('',#3116,.T.);
#2478=FACE_OUTER_BOUND('',#3117,.T.);
#2479=FACE_OUTER_BOUND('',#3118,.T.);
#2480=FACE_OUTER_BOUND('',#3119,.T.);
#2481=FACE_OUTER_BOUND('',#3120,.T.);
#2482=FACE_OUTER_BOUND('',#3121,.T.);
#2483=FACE_OUTER_BOUND('',#3122,.T.);
#2484=FACE_OUTER_BOUND('',#3123,.T.);
#2485=FACE_OUTER_BOUND('',#3124,.T.);
#2486=FACE_OUTER_BOUND('',#3125,.T.);
#2487=FACE_OUTER_BOUND('',#3126,.T.);
#2488=FACE_OUTER_BOUND('',#3127,.T.);
#2489=FACE_OUTER_BOUND('',#3128,.T.);
#2490=FACE_OUTER_BOUND('',#3150,.T.);
#2491=FACE_OUTER_BOUND('',#3151,.T.);
#2492=FACE_OUTER_BOUND('',#3152,.T.);
#2493=FACE_OUTER_BOUND('',#3153,.T.);
#2494=FACE_OUTER_BOUND('',#3154,.T.);
#2495=FACE_OUTER_BOUND('',#3155,.T.);
#2496=FACE_OUTER_BOUND('',#3156,.T.);
#2497=FACE_OUTER_BOUND('',#3157,.T.);
#2498=FACE_OUTER_BOUND('',#3158,.T.);
#2499=FACE_OUTER_BOUND('',#3159,.T.);
#2500=FACE_OUTER_BOUND('',#3161,.T.);
#2501=FACE_OUTER_BOUND('',#3162,.T.);
#2502=FACE_OUTER_BOUND('',#3163,.T.);
#2503=FACE_OUTER_BOUND('',#3164,.T.);
#2504=FACE_OUTER_BOUND('',#3165,.T.);
#2505=FACE_OUTER_BOUND('',#3166,.T.);
#2506=FACE_OUTER_BOUND('',#3167,.T.);
#2507=FACE_OUTER_BOUND('',#3168,.T.);
#2508=FACE_OUTER_BOUND('',#3169,.T.);
#2509=FACE_OUTER_BOUND('',#3170,.T.);
#2510=FACE_OUTER_BOUND('',#3171,.T.);
#2511=FACE_OUTER_BOUND('',#3172,.T.);
#2512=FACE_OUTER_BOUND('',#3173,.T.);
#2513=FACE_OUTER_BOUND('',#3174,.T.);
#2514=FACE_OUTER_BOUND('',#3175,.T.);
#2515=FACE_OUTER_BOUND('',#3176,.T.);
#2516=FACE_OUTER_BOUND('',#3177,.T.);
#2517=FACE_OUTER_BOUND('',#3178,.T.);
#2518=FACE_OUTER_BOUND('',#3179,.T.);
#2519=FACE_OUTER_BOUND('',#3180,.T.);
#2520=FACE_OUTER_BOUND('',#3181,.T.);
#2521=FACE_OUTER_BOUND('',#3182,.T.);
#2522=FACE_OUTER_BOUND('',#3183,.T.);
#2523=FACE_OUTER_BOUND('',#3184,.T.);
#2524=FACE_OUTER_BOUND('',#3185,.T.);
#2525=FACE_OUTER_BOUND('',#3186,.T.);
#2526=FACE_OUTER_BOUND('',#3187,.T.);
#2527=FACE_OUTER_BOUND('',#3188,.T.);
#2528=FACE_OUTER_BOUND('',#3189,.T.);
#2529=FACE_OUTER_BOUND('',#3190,.T.);
#2530=FACE_OUTER_BOUND('',#3191,.T.);
#2531=FACE_OUTER_BOUND('',#3193,.T.);
#2532=FACE_OUTER_BOUND('',#3194,.T.);
#2533=FACE_OUTER_BOUND('',#3195,.T.);
#2534=FACE_OUTER_BOUND('',#3196,.T.);
#2535=FACE_OUTER_BOUND('',#3197,.T.);
#2536=FACE_OUTER_BOUND('',#3198,.T.);
#2537=FACE_OUTER_BOUND('',#3199,.T.);
#2538=FACE_OUTER_BOUND('',#3200,.T.);
#2539=FACE_OUTER_BOUND('',#3201,.T.);
#2540=FACE_OUTER_BOUND('',#3202,.T.);
#2541=FACE_OUTER_BOUND('',#3204,.T.);
#2542=FACE_OUTER_BOUND('',#3205,.T.);
#2543=FACE_OUTER_BOUND('',#3206,.T.);
#2544=FACE_OUTER_BOUND('',#3207,.T.);
#2545=FACE_OUTER_BOUND('',#3208,.T.);
#2546=FACE_OUTER_BOUND('',#3209,.T.);
#2547=FACE_OUTER_BOUND('',#3210,.T.);
#2548=FACE_OUTER_BOUND('',#3211,.T.);
#2549=FACE_OUTER_BOUND('',#3212,.T.);
#2550=FACE_OUTER_BOUND('',#3213,.T.);
#2551=FACE_OUTER_BOUND('',#3214,.T.);
#2552=FACE_OUTER_BOUND('',#3215,.T.);
#2553=FACE_OUTER_BOUND('',#3216,.T.);
#2554=FACE_OUTER_BOUND('',#3218,.T.);
#2555=FACE_OUTER_BOUND('',#3219,.T.);
#2556=FACE_OUTER_BOUND('',#3220,.T.);
#2557=FACE_OUTER_BOUND('',#3221,.T.);
#2558=FACE_OUTER_BOUND('',#3222,.T.);
#2559=FACE_OUTER_BOUND('',#3223,.T.);
#2560=FACE_OUTER_BOUND('',#3224,.T.);
#2561=FACE_OUTER_BOUND('',#3225,.T.);
#2562=FACE_OUTER_BOUND('',#3226,.T.);
#2563=FACE_OUTER_BOUND('',#3227,.T.);
#2564=FACE_OUTER_BOUND('',#3228,.T.);
#2565=FACE_OUTER_BOUND('',#3229,.T.);
#2566=FACE_OUTER_BOUND('',#3230,.T.);
#2567=FACE_OUTER_BOUND('',#3231,.T.);
#2568=FACE_OUTER_BOUND('',#3232,.T.);
#2569=FACE_OUTER_BOUND('',#3233,.T.);
#2570=FACE_OUTER_BOUND('',#3234,.T.);
#2571=FACE_OUTER_BOUND('',#3235,.T.);
#2572=FACE_OUTER_BOUND('',#3236,.T.);
#2573=FACE_OUTER_BOUND('',#3237,.T.);
#2574=FACE_OUTER_BOUND('',#3238,.T.);
#2575=FACE_OUTER_BOUND('',#3239,.T.);
#2576=FACE_OUTER_BOUND('',#3240,.T.);
#2577=FACE_OUTER_BOUND('',#3241,.T.);
#2578=FACE_OUTER_BOUND('',#3242,.T.);
#2579=FACE_OUTER_BOUND('',#3243,.T.);
#2580=FACE_OUTER_BOUND('',#3244,.T.);
#2581=FACE_OUTER_BOUND('',#3245,.T.);
#2582=FACE_OUTER_BOUND('',#3246,.T.);
#2583=FACE_OUTER_BOUND('',#3247,.T.);
#2584=FACE_OUTER_BOUND('',#3248,.T.);
#2585=FACE_OUTER_BOUND('',#3250,.T.);
#2586=FACE_OUTER_BOUND('',#3251,.T.);
#2587=FACE_OUTER_BOUND('',#3252,.T.);
#2588=FACE_OUTER_BOUND('',#3253,.T.);
#2589=FACE_OUTER_BOUND('',#3254,.T.);
#2590=FACE_OUTER_BOUND('',#3255,.T.);
#2591=FACE_OUTER_BOUND('',#3256,.T.);
#2592=FACE_OUTER_BOUND('',#3257,.T.);
#2593=FACE_OUTER_BOUND('',#3258,.T.);
#2594=FACE_OUTER_BOUND('',#3259,.T.);
#2595=FACE_OUTER_BOUND('',#3260,.T.);
#2596=FACE_OUTER_BOUND('',#3261,.T.);
#2597=FACE_OUTER_BOUND('',#3262,.T.);
#2598=FACE_OUTER_BOUND('',#3263,.T.);
#2599=FACE_OUTER_BOUND('',#3264,.T.);
#2600=FACE_OUTER_BOUND('',#3265,.T.);
#2601=FACE_OUTER_BOUND('',#3267,.T.);
#2602=FACE_OUTER_BOUND('',#3268,.T.);
#2603=FACE_OUTER_BOUND('',#3269,.T.);
#2604=FACE_OUTER_BOUND('',#3270,.T.);
#2605=FACE_OUTER_BOUND('',#3271,.T.);
#2606=FACE_OUTER_BOUND('',#3272,.T.);
#2607=FACE_OUTER_BOUND('',#3273,.T.);
#2608=FACE_OUTER_BOUND('',#3274,.T.);
#2609=FACE_OUTER_BOUND('',#3275,.T.);
#2610=FACE_OUTER_BOUND('',#3276,.T.);
#2611=FACE_OUTER_BOUND('',#3277,.T.);
#2612=FACE_OUTER_BOUND('',#3278,.T.);
#2613=FACE_OUTER_BOUND('',#3279,.T.);
#2614=FACE_OUTER_BOUND('',#3280,.T.);
#2615=FACE_OUTER_BOUND('',#3281,.T.);
#2616=FACE_OUTER_BOUND('',#3282,.T.);
#2617=FACE_OUTER_BOUND('',#3283,.T.);
#2618=FACE_OUTER_BOUND('',#3284,.T.);
#2619=FACE_OUTER_BOUND('',#3285,.T.);
#2620=FACE_OUTER_BOUND('',#3286,.T.);
#2621=FACE_OUTER_BOUND('',#3287,.T.);
#2622=FACE_OUTER_BOUND('',#3288,.T.);
#2623=FACE_OUTER_BOUND('',#3289,.T.);
#2624=FACE_OUTER_BOUND('',#3290,.T.);
#2625=FACE_OUTER_BOUND('',#3291,.T.);
#2626=FACE_OUTER_BOUND('',#3292,.T.);
#2627=FACE_OUTER_BOUND('',#3293,.T.);
#2628=FACE_OUTER_BOUND('',#3294,.T.);
#2629=FACE_OUTER_BOUND('',#3295,.T.);
#2630=FACE_OUTER_BOUND('',#3296,.T.);
#2631=FACE_OUTER_BOUND('',#3297,.T.);
#2632=FACE_OUTER_BOUND('',#3299,.T.);
#2633=FACE_OUTER_BOUND('',#3300,.T.);
#2634=FACE_OUTER_BOUND('',#3301,.T.);
#2635=FACE_OUTER_BOUND('',#3302,.T.);
#2636=FACE_OUTER_BOUND('',#3303,.T.);
#2637=FACE_OUTER_BOUND('',#3304,.T.);
#2638=FACE_OUTER_BOUND('',#3305,.T.);
#2639=FACE_OUTER_BOUND('',#3306,.T.);
#2640=FACE_OUTER_BOUND('',#3307,.T.);
#2641=EDGE_LOOP('',(#6103));
#2642=EDGE_LOOP('',(#6104));
#2643=EDGE_LOOP('',(#6105,#6106,#6107,#6108));
#2644=EDGE_LOOP('',(#6109,#6110,#6111,#6112));
#2645=EDGE_LOOP('',(#6113));
#2646=EDGE_LOOP('',(#6114,#6115,#6116,#6117));
#2647=EDGE_LOOP('',(#6118,#6119,#6120,#6121));
#2648=EDGE_LOOP('',(#6122));
#2649=EDGE_LOOP('',(#6123,#6124,#6125,#6126,#6127,#6128));
#2650=EDGE_LOOP('',(#6129,#6130,#6131,#6132,#6133,#6134));
#2651=EDGE_LOOP('',(#6135,#6136,#6137,#6138));
#2652=EDGE_LOOP('',(#6139,#6140,#6141,#6142));
#2653=EDGE_LOOP('',(#6143,#6144,#6145,#6146));
#2654=EDGE_LOOP('',(#6147,#6148,#6149,#6150));
#2655=EDGE_LOOP('',(#6151,#6152,#6153,#6154));
#2656=EDGE_LOOP('',(#6155,#6156,#6157,#6158));
#2657=EDGE_LOOP('',(#6159,#6160,#6161,#6162));
#2658=EDGE_LOOP('',(#6163,#6164,#6165,#6166,#6167,#6168,#6169,#6170,#6171,
#6172,#6173,#6174,#6175,#6176,#6177,#6178,#6179,#6180,#6181,#6182,#6183,
#6184,#6185,#6186));
#2659=EDGE_LOOP('',(#6187,#6188,#6189,#6190,#6191,#6192));
#2660=EDGE_LOOP('',(#6193,#6194,#6195,#6196,#6197,#6198));
#2661=EDGE_LOOP('',(#6199,#6200,#6201,#6202));
#2662=EDGE_LOOP('',(#6203,#6204,#6205,#6206));
#2663=EDGE_LOOP('',(#6207,#6208,#6209,#6210,#6211,#6212,#6213,#6214,#6215,
#6216,#6217,#6218,#6219,#6220,#6221,#6222,#6223,#6224,#6225,#6226,#6227,
#6228,#6229,#6230));
#2664=EDGE_LOOP('',(#6231,#6232,#6233,#6234));
#2665=EDGE_LOOP('',(#6235,#6236,#6237,#6238));
#2666=EDGE_LOOP('',(#6239,#6240,#6241,#6242));
#2667=EDGE_LOOP('',(#6243,#6244,#6245,#6246));
#2668=EDGE_LOOP('',(#6247,#6248,#6249));
#2669=EDGE_LOOP('',(#6250,#6251,#6252));
#2670=EDGE_LOOP('',(#6253,#6254,#6255,#6256));
#2671=EDGE_LOOP('',(#6257,#6258,#6259));
#2672=EDGE_LOOP('',(#6260,#6261,#6262,#6263));
#2673=EDGE_LOOP('',(#6264,#6265,#6266,#6267));
#2674=EDGE_LOOP('',(#6268,#6269,#6270));
#2675=EDGE_LOOP('',(#6271,#6272,#6273,#6274));
#2676=EDGE_LOOP('',(#6275,#6276,#6277,#6278));
#2677=EDGE_LOOP('',(#6279,#6280,#6281,#6282));
#2678=EDGE_LOOP('',(#6283,#6284,#6285));
#2679=EDGE_LOOP('',(#6286,#6287,#6288,#6289));
#2680=EDGE_LOOP('',(#6290,#6291,#6292,#6293));
#2681=EDGE_LOOP('',(#6294,#6295,#6296,#6297));
#2682=EDGE_LOOP('',(#6298,#6299,#6300));
#2683=EDGE_LOOP('',(#6301,#6302,#6303,#6304));
#2684=EDGE_LOOP('',(#6305,#6306,#6307,#6308));
#2685=EDGE_LOOP('',(#6309,#6310,#6311,#6312));
#2686=EDGE_LOOP('',(#6313,#6314,#6315,#6316));
#2687=EDGE_LOOP('',(#6317,#6318,#6319));
#2688=EDGE_LOOP('',(#6320,#6321,#6322));
#2689=EDGE_LOOP('',(#6323,#6324,#6325,#6326));
#2690=EDGE_LOOP('',(#6327,#6328,#6329));
#2691=EDGE_LOOP('',(#6330,#6331,#6332,#6333));
#2692=EDGE_LOOP('',(#6334,#6335,#6336,#6337));
#2693=EDGE_LOOP('',(#6338,#6339,#6340));
#2694=EDGE_LOOP('',(#6341,#6342,#6343,#6344));
#2695=EDGE_LOOP('',(#6345,#6346,#6347,#6348));
#2696=EDGE_LOOP('',(#6349,#6350,#6351,#6352));
#2697=EDGE_LOOP('',(#6353,#6354,#6355));
#2698=EDGE_LOOP('',(#6356,#6357,#6358,#6359));
#2699=EDGE_LOOP('',(#6360,#6361,#6362,#6363));
#2700=EDGE_LOOP('',(#6364,#6365,#6366));
#2701=EDGE_LOOP('',(#6367,#6368,#6369,#6370));
#2702=EDGE_LOOP('',(#6371,#6372,#6373));
#2703=EDGE_LOOP('',(#6374,#6375,#6376,#6377));
#2704=EDGE_LOOP('',(#6378,#6379,#6380,#6381));
#2705=EDGE_LOOP('',(#6382,#6383,#6384));
#2706=EDGE_LOOP('',(#6385,#6386,#6387,#6388));
#2707=EDGE_LOOP('',(#6389,#6390,#6391,#6392));
#2708=EDGE_LOOP('',(#6393,#6394,#6395,#6396));
#2709=EDGE_LOOP('',(#6397,#6398,#6399,#6400));
#2710=EDGE_LOOP('',(#6401,#6402,#6403,#6404));
#2711=EDGE_LOOP('',(#6405,#6406,#6407,#6408));
#2712=EDGE_LOOP('',(#6409,#6410,#6411,#6412));
#2713=EDGE_LOOP('',(#6413,#6414,#6415,#6416));
#2714=EDGE_LOOP('',(#6417,#6418,#6419,#6420));
#2715=EDGE_LOOP('',(#6421,#6422,#6423,#6424));
#2716=EDGE_LOOP('',(#6425,#6426,#6427,#6428));
#2717=EDGE_LOOP('',(#6429,#6430,#6431,#6432));
#2718=EDGE_LOOP('',(#6433,#6434,#6435,#6436));
#2719=EDGE_LOOP('',(#6437,#6438,#6439,#6440));
#2720=EDGE_LOOP('',(#6441,#6442,#6443,#6444));
#2721=EDGE_LOOP('',(#6445,#6446,#6447,#6448));
#2722=EDGE_LOOP('',(#6449,#6450,#6451,#6452));
#2723=EDGE_LOOP('',(#6453,#6454,#6455,#6456));
#2724=EDGE_LOOP('',(#6457,#6458,#6459,#6460));
#2725=EDGE_LOOP('',(#6461,#6462,#6463,#6464));
#2726=EDGE_LOOP('',(#6465,#6466,#6467,#6468));
#2727=EDGE_LOOP('',(#6469,#6470,#6471,#6472));
#2728=EDGE_LOOP('',(#6473,#6474,#6475,#6476));
#2729=EDGE_LOOP('',(#6477,#6478,#6479,#6480));
#2730=EDGE_LOOP('',(#6481,#6482,#6483,#6484));
#2731=EDGE_LOOP('',(#6485,#6486,#6487,#6488));
#2732=EDGE_LOOP('',(#6489,#6490,#6491,#6492));
#2733=EDGE_LOOP('',(#6493,#6494,#6495,#6496));
#2734=EDGE_LOOP('',(#6497));
#2735=EDGE_LOOP('',(#6498,#6499,#6500,#6501));
#2736=EDGE_LOOP('',(#6502));
#2737=EDGE_LOOP('',(#6503,#6504,#6505,#6506));
#2738=EDGE_LOOP('',(#6507,#6508,#6509));
#2739=EDGE_LOOP('',(#6510,#6511,#6512));
#2740=EDGE_LOOP('',(#6513,#6514,#6515,#6516));
#2741=EDGE_LOOP('',(#6517,#6518,#6519,#6520));
#2742=EDGE_LOOP('',(#6521,#6522,#6523,#6524));
#2743=EDGE_LOOP('',(#6525,#6526,#6527,#6528));
#2744=EDGE_LOOP('',(#6529,#6530,#6531,#6532));
#2745=EDGE_LOOP('',(#6533,#6534,#6535,#6536));
#2746=EDGE_LOOP('',(#6537,#6538,#6539));
#2747=EDGE_LOOP('',(#6540,#6541,#6542,#6543));
#2748=EDGE_LOOP('',(#6544,#6545,#6546));
#2749=EDGE_LOOP('',(#6547,#6548,#6549,#6550));
#2750=EDGE_LOOP('',(#6551,#6552,#6553));
#2751=EDGE_LOOP('',(#6554,#6555,#6556));
#2752=EDGE_LOOP('',(#6557,#6558,#6559,#6560));
#2753=EDGE_LOOP('',(#6561,#6562,#6563));
#2754=EDGE_LOOP('',(#6564,#6565,#6566,#6567));
#2755=EDGE_LOOP('',(#6568,#6569,#6570));
#2756=EDGE_LOOP('',(#6571,#6572,#6573,#6574));
#2757=EDGE_LOOP('',(#6575,#6576,#6577));
#2758=EDGE_LOOP('',(#6578,#6579,#6580));
#2759=EDGE_LOOP('',(#6581,#6582,#6583,#6584));
#2760=EDGE_LOOP('',(#6585,#6586,#6587,#6588));
#2761=EDGE_LOOP('',(#6589,#6590,#6591,#6592));
#2762=EDGE_LOOP('',(#6593,#6594,#6595));
#2763=EDGE_LOOP('',(#6596,#6597,#6598,#6599));
#2764=EDGE_LOOP('',(#6600,#6601,#6602));
#2765=EDGE_LOOP('',(#6603,#6604,#6605));
#2766=EDGE_LOOP('',(#6606,#6607,#6608,#6609));
#2767=EDGE_LOOP('',(#6610,#6611,#6612));
#2768=EDGE_LOOP('',(#6613,#6614,#6615));
#2769=EDGE_LOOP('',(#6616,#6617,#6618));
#2770=EDGE_LOOP('',(#6619,#6620,#6621,#6622));
#2771=EDGE_LOOP('',(#6623,#6624,#6625,#6626));
#2772=EDGE_LOOP('',(#6627,#6628,#6629,#6630));
#2773=EDGE_LOOP('',(#6631,#6632,#6633,#6634));
#2774=EDGE_LOOP('',(#6635,#6636,#6637,#6638));
#2775=EDGE_LOOP('',(#6639,#6640,#6641,#6642));
#2776=EDGE_LOOP('',(#6643,#6644,#6645,#6646));
#2777=EDGE_LOOP('',(#6647,#6648,#6649,#6650));
#2778=EDGE_LOOP('',(#6651,#6652,#6653,#6654));
#2779=EDGE_LOOP('',(#6655,#6656,#6657,#6658));
#2780=EDGE_LOOP('',(#6659,#6660,#6661,#6662));
#2781=EDGE_LOOP('',(#6663,#6664,#6665,#6666));
#2782=EDGE_LOOP('',(#6667,#6668,#6669,#6670));
#2783=EDGE_LOOP('',(#6671,#6672,#6673,#6674));
#2784=EDGE_LOOP('',(#6675,#6676,#6677,#6678));
#2785=EDGE_LOOP('',(#6679,#6680,#6681,#6682));
#2786=EDGE_LOOP('',(#6683,#6684,#6685,#6686));
#2787=EDGE_LOOP('',(#6687,#6688,#6689,#6690));
#2788=EDGE_LOOP('',(#6691,#6692,#6693,#6694));
#2789=EDGE_LOOP('',(#6695,#6696,#6697,#6698));
#2790=EDGE_LOOP('',(#6699,#6700,#6701,#6702));
#2791=EDGE_LOOP('',(#6703,#6704,#6705,#6706));
#2792=EDGE_LOOP('',(#6707,#6708,#6709,#6710));
#2793=EDGE_LOOP('',(#6711,#6712,#6713,#6714));
#2794=EDGE_LOOP('',(#6715,#6716,#6717,#6718));
#2795=EDGE_LOOP('',(#6719,#6720,#6721,#6722));
#2796=EDGE_LOOP('',(#6723,#6724,#6725,#6726));
#2797=EDGE_LOOP('',(#6727,#6728,#6729,#6730));
#2798=EDGE_LOOP('',(#6731,#6732,#6733,#6734,#6735,#6736,#6737,#6738,#6739,
#6740,#6741,#6742,#6743,#6744,#6745,#6746));
#2799=EDGE_LOOP('',(#6747,#6748,#6749,#6750));
#2800=EDGE_LOOP('',(#6751,#6752,#6753,#6754));
#2801=EDGE_LOOP('',(#6755));
#2802=EDGE_LOOP('',(#6756));
#2803=EDGE_LOOP('',(#6757,#6758,#6759,#6760));
#2804=EDGE_LOOP('',(#6761,#6762,#6763,#6764));
#2805=EDGE_LOOP('',(#6765,#6766,#6767,#6768));
#2806=EDGE_LOOP('',(#6769,#6770,#6771,#6772));
#2807=EDGE_LOOP('',(#6773,#6774,#6775,#6776));
#2808=EDGE_LOOP('',(#6777,#6778,#6779,#6780));
#2809=EDGE_LOOP('',(#6781));
#2810=EDGE_LOOP('',(#6782));
#2811=EDGE_LOOP('',(#6783));
#2812=EDGE_LOOP('',(#6784));
#2813=EDGE_LOOP('',(#6785,#6786,#6787,#6788));
#2814=EDGE_LOOP('',(#6789,#6790,#6791,#6792));
#2815=EDGE_LOOP('',(#6793,#6794,#6795,#6796));
#2816=EDGE_LOOP('',(#6797,#6798,#6799,#6800));
#2817=EDGE_LOOP('',(#6801,#6802,#6803,#6804,#6805,#6806,#6807,#6808,#6809,
#6810,#6811,#6812,#6813,#6814,#6815,#6816));
#2818=EDGE_LOOP('',(#6817,#6818,#6819,#6820));
#2819=EDGE_LOOP('',(#6821));
#2820=EDGE_LOOP('',(#6822,#6823,#6824,#6825));
#2821=EDGE_LOOP('',(#6826));
#2822=EDGE_LOOP('',(#6827,#6828,#6829,#6830));
#2823=EDGE_LOOP('',(#6831));
#2824=EDGE_LOOP('',(#6832,#6833,#6834,#6835));
#2825=EDGE_LOOP('',(#6836));
#2826=EDGE_LOOP('',(#6837,#6838,#6839,#6840));
#2827=EDGE_LOOP('',(#6841));
#2828=EDGE_LOOP('',(#6842,#6843,#6844,#6845));
#2829=EDGE_LOOP('',(#6846));
#2830=EDGE_LOOP('',(#6847,#6848,#6849,#6850));
#2831=EDGE_LOOP('',(#6851));
#2832=EDGE_LOOP('',(#6852,#6853,#6854,#6855));
#2833=EDGE_LOOP('',(#6856));
#2834=EDGE_LOOP('',(#6857,#6858,#6859,#6860,#6861,#6862));
#2835=EDGE_LOOP('',(#6863,#6864,#6865,#6866,#6867,#6868));
#2836=EDGE_LOOP('',(#6869,#6870,#6871,#6872));
#2837=EDGE_LOOP('',(#6873,#6874,#6875,#6876));
#2838=EDGE_LOOP('',(#6877,#6878,#6879,#6880));
#2839=EDGE_LOOP('',(#6881,#6882,#6883,#6884));
#2840=EDGE_LOOP('',(#6885,#6886,#6887,#6888));
#2841=EDGE_LOOP('',(#6889));
#2842=EDGE_LOOP('',(#6890));
#2843=EDGE_LOOP('',(#6891));
#2844=EDGE_LOOP('',(#6892));
#2845=EDGE_LOOP('',(#6893,#6894,#6895,#6896));
#2846=EDGE_LOOP('',(#6897,#6898,#6899,#6900));
#2847=EDGE_LOOP('',(#6901,#6902,#6903,#6904,#6905,#6906,#6907,#6908,#6909,
#6910,#6911,#6912,#6913,#6914,#6915,#6916,#6917,#6918,#6919,#6920,#6921,
#6922,#6923,#6924));
#2848=EDGE_LOOP('',(#6925,#6926,#6927,#6928,#6929,#6930));
#2849=EDGE_LOOP('',(#6931,#6932,#6933,#6934,#6935,#6936));
#2850=EDGE_LOOP('',(#6937,#6938,#6939,#6940));
#2851=EDGE_LOOP('',(#6941,#6942,#6943,#6944));
#2852=EDGE_LOOP('',(#6945,#6946,#6947,#6948,#6949,#6950,#6951,#6952,#6953,
#6954,#6955,#6956,#6957,#6958,#6959,#6960,#6961,#6962,#6963,#6964,#6965,
#6966,#6967,#6968));
#2853=EDGE_LOOP('',(#6969,#6970,#6971,#6972));
#2854=EDGE_LOOP('',(#6973));
#2855=EDGE_LOOP('',(#6974));
#2856=EDGE_LOOP('',(#6975));
#2857=EDGE_LOOP('',(#6976));
#2858=EDGE_LOOP('',(#6977,#6978,#6979,#6980));
#2859=EDGE_LOOP('',(#6981,#6982,#6983,#6984));
#2860=EDGE_LOOP('',(#6985,#6986,#6987,#6988));
#2861=EDGE_LOOP('',(#6989,#6990,#6991));
#2862=EDGE_LOOP('',(#6992,#6993,#6994));
#2863=EDGE_LOOP('',(#6995,#6996,#6997,#6998));
#2864=EDGE_LOOP('',(#6999,#7000,#7001));
#2865=EDGE_LOOP('',(#7002,#7003,#7004,#7005));
#2866=EDGE_LOOP('',(#7006,#7007,#7008,#7009));
#2867=EDGE_LOOP('',(#7010,#7011,#7012));
#2868=EDGE_LOOP('',(#7013,#7014,#7015,#7016));
#2869=EDGE_LOOP('',(#7017,#7018,#7019,#7020));
#2870=EDGE_LOOP('',(#7021,#7022,#7023,#7024));
#2871=EDGE_LOOP('',(#7025,#7026,#7027));
#2872=EDGE_LOOP('',(#7028,#7029,#7030,#7031));
#2873=EDGE_LOOP('',(#7032,#7033,#7034,#7035));
#2874=EDGE_LOOP('',(#7036,#7037,#7038,#7039));
#2875=EDGE_LOOP('',(#7040,#7041,#7042));
#2876=EDGE_LOOP('',(#7043,#7044,#7045,#7046));
#2877=EDGE_LOOP('',(#7047,#7048,#7049,#7050));
#2878=EDGE_LOOP('',(#7051,#7052,#7053,#7054));
#2879=EDGE_LOOP('',(#7055,#7056,#7057,#7058));
#2880=EDGE_LOOP('',(#7059,#7060,#7061));
#2881=EDGE_LOOP('',(#7062,#7063,#7064));
#2882=EDGE_LOOP('',(#7065,#7066,#7067,#7068));
#2883=EDGE_LOOP('',(#7069,#7070,#7071));
#2884=EDGE_LOOP('',(#7072,#7073,#7074,#7075));
#2885=EDGE_LOOP('',(#7076,#7077,#7078,#7079));
#2886=EDGE_LOOP('',(#7080,#7081,#7082));
#2887=EDGE_LOOP('',(#7083,#7084,#7085,#7086));
#2888=EDGE_LOOP('',(#7087,#7088,#7089,#7090));
#2889=EDGE_LOOP('',(#7091,#7092,#7093,#7094));
#2890=EDGE_LOOP('',(#7095,#7096,#7097));
#2891=EDGE_LOOP('',(#7098,#7099,#7100,#7101));
#2892=EDGE_LOOP('',(#7102,#7103,#7104,#7105));
#2893=EDGE_LOOP('',(#7106,#7107,#7108));
#2894=EDGE_LOOP('',(#7109,#7110,#7111,#7112));
#2895=EDGE_LOOP('',(#7113,#7114,#7115));
#2896=EDGE_LOOP('',(#7116,#7117,#7118,#7119));
#2897=EDGE_LOOP('',(#7120,#7121,#7122,#7123));
#2898=EDGE_LOOP('',(#7124,#7125,#7126));
#2899=EDGE_LOOP('',(#7127,#7128,#7129,#7130));
#2900=EDGE_LOOP('',(#7131,#7132,#7133,#7134));
#2901=EDGE_LOOP('',(#7135,#7136,#7137,#7138));
#2902=EDGE_LOOP('',(#7139,#7140,#7141,#7142));
#2903=EDGE_LOOP('',(#7143,#7144,#7145,#7146));
#2904=EDGE_LOOP('',(#7147,#7148,#7149,#7150));
#2905=EDGE_LOOP('',(#7151,#7152,#7153,#7154));
#2906=EDGE_LOOP('',(#7155,#7156,#7157,#7158));
#2907=EDGE_LOOP('',(#7159,#7160,#7161,#7162));
#2908=EDGE_LOOP('',(#7163,#7164,#7165,#7166));
#2909=EDGE_LOOP('',(#7167,#7168,#7169,#7170));
#2910=EDGE_LOOP('',(#7171,#7172,#7173,#7174));
#2911=EDGE_LOOP('',(#7175,#7176,#7177,#7178));
#2912=EDGE_LOOP('',(#7179,#7180,#7181,#7182));
#2913=EDGE_LOOP('',(#7183,#7184,#7185,#7186));
#2914=EDGE_LOOP('',(#7187,#7188,#7189,#7190));
#2915=EDGE_LOOP('',(#7191,#7192,#7193,#7194));
#2916=EDGE_LOOP('',(#7195,#7196,#7197,#7198));
#2917=EDGE_LOOP('',(#7199,#7200,#7201,#7202));
#2918=EDGE_LOOP('',(#7203,#7204,#7205,#7206));
#2919=EDGE_LOOP('',(#7207,#7208,#7209,#7210));
#2920=EDGE_LOOP('',(#7211,#7212,#7213,#7214));
#2921=EDGE_LOOP('',(#7215,#7216,#7217,#7218));
#2922=EDGE_LOOP('',(#7219,#7220,#7221,#7222));
#2923=EDGE_LOOP('',(#7223,#7224,#7225,#7226));
#2924=EDGE_LOOP('',(#7227,#7228,#7229,#7230));
#2925=EDGE_LOOP('',(#7231,#7232,#7233,#7234));
#2926=EDGE_LOOP('',(#7235,#7236,#7237,#7238));
#2927=EDGE_LOOP('',(#7239,#7240,#7241,#7242));
#2928=EDGE_LOOP('',(#7243,#7244,#7245,#7246));
#2929=EDGE_LOOP('',(#7247,#7248,#7249,#7250));
#2930=EDGE_LOOP('',(#7251,#7252,#7253,#7254));
#2931=EDGE_LOOP('',(#7255,#7256,#7257,#7258));
#2932=EDGE_LOOP('',(#7259,#7260,#7261,#7262));
#2933=EDGE_LOOP('',(#7263,#7264,#7265,#7266));
#2934=EDGE_LOOP('',(#7267,#7268,#7269));
#2935=EDGE_LOOP('',(#7270,#7271,#7272,#7273));
#2936=EDGE_LOOP('',(#7274,#7275,#7276,#7277));
#2937=EDGE_LOOP('',(#7278,#7279,#7280));
#2938=EDGE_LOOP('',(#7281,#7282,#7283));
#2939=EDGE_LOOP('',(#7284,#7285,#7286,#7287));
#2940=EDGE_LOOP('',(#7288,#7289,#7290));
#2941=EDGE_LOOP('',(#7291,#7292,#7293));
#2942=EDGE_LOOP('',(#7294,#7295,#7296));
#2943=EDGE_LOOP('',(#7297,#7298,#7299));
#2944=EDGE_LOOP('',(#7300,#7301,#7302,#7303));
#2945=EDGE_LOOP('',(#7304,#7305,#7306));
#2946=EDGE_LOOP('',(#7307,#7308,#7309,#7310));
#2947=EDGE_LOOP('',(#7311,#7312,#7313,#7314));
#2948=EDGE_LOOP('',(#7315,#7316,#7317,#7318));
#2949=EDGE_LOOP('',(#7319,#7320,#7321,#7322));
#2950=EDGE_LOOP('',(#7323,#7324,#7325,#7326));
#2951=EDGE_LOOP('',(#7327,#7328,#7329,#7330));
#2952=EDGE_LOOP('',(#7331,#7332,#7333,#7334));
#2953=EDGE_LOOP('',(#7335,#7336,#7337,#7338));
#2954=EDGE_LOOP('',(#7339,#7340,#7341,#7342));
#2955=EDGE_LOOP('',(#7343,#7344,#7345,#7346));
#2956=EDGE_LOOP('',(#7347,#7348,#7349,#7350));
#2957=EDGE_LOOP('',(#7351,#7352,#7353,#7354));
#2958=EDGE_LOOP('',(#7355,#7356,#7357,#7358));
#2959=EDGE_LOOP('',(#7359,#7360,#7361,#7362));
#2960=EDGE_LOOP('',(#7363,#7364,#7365,#7366));
#2961=EDGE_LOOP('',(#7367,#7368,#7369,#7370,#7371,#7372,#7373));
#2962=EDGE_LOOP('',(#7374,#7375,#7376,#7377));
#2963=EDGE_LOOP('',(#7378,#7379,#7380,#7381));
#2964=EDGE_LOOP('',(#7382,#7383,#7384,#7385));
#2965=EDGE_LOOP('',(#7386,#7387,#7388,#7389));
#2966=EDGE_LOOP('',(#7390,#7391,#7392,#7393,#7394,#7395,#7396));
#2967=EDGE_LOOP('',(#7397,#7398,#7399,#7400));
#2968=EDGE_LOOP('',(#7401,#7402,#7403,#7404));
#2969=EDGE_LOOP('',(#7405,#7406,#7407,#7408));
#2970=EDGE_LOOP('',(#7409,#7410,#7411,#7412));
#2971=EDGE_LOOP('',(#7413,#7414,#7415,#7416));
#2972=EDGE_LOOP('',(#7417,#7418,#7419,#7420));
#2973=EDGE_LOOP('',(#7421,#7422,#7423,#7424));
#2974=EDGE_LOOP('',(#7425,#7426,#7427,#7428));
#2975=EDGE_LOOP('',(#7429,#7430,#7431,#7432,#7433,#7434,#7435,#7436,#7437,
#7438,#7439,#7440));
#2976=EDGE_LOOP('',(#7441,#7442,#7443,#7444,#7445,#7446,#7447,#7448,#7449,
#7450,#7451,#7452,#7453,#7454,#7455,#7456,#7457,#7458,#7459,#7460,#7461,
#7462,#7463,#7464,#7465));
#2977=EDGE_LOOP('',(#7466,#7467,#7468,#7469));
#2978=EDGE_LOOP('',(#7470,#7471,#7472,#7473));
#2979=EDGE_LOOP('',(#7474,#7475,#7476,#7477));
#2980=EDGE_LOOP('',(#7478,#7479,#7480,#7481,#7482,#7483,#7484,#7485,#7486,
#7487,#7488,#7489));
#2981=EDGE_LOOP('',(#7490,#7491,#7492,#7493));
#2982=EDGE_LOOP('',(#7494,#7495,#7496,#7497));
#2983=EDGE_LOOP('',(#7498,#7499,#7500,#7501,#7502,#7503,#7504,#7505,#7506,
#7507,#7508,#7509));
#2984=EDGE_LOOP('',(#7510,#7511,#7512,#7513));
#2985=EDGE_LOOP('',(#7514,#7515,#7516,#7517,#7518,#7519,#7520,#7521,#7522,
#7523,#7524,#7525));
#2986=EDGE_LOOP('',(#7526,#7527,#7528,#7529));
#2987=EDGE_LOOP('',(#7530,#7531,#7532,#7533,#7534,#7535,#7536,#7537,#7538,
#7539,#7540,#7541));
#2988=EDGE_LOOP('',(#7542,#7543,#7544,#7545));
#2989=EDGE_LOOP('',(#7546,#7547,#7548,#7549,#7550,#7551,#7552,#7553,#7554,
#7555,#7556,#7557));
#2990=EDGE_LOOP('',(#7558,#7559,#7560,#7561));
#2991=EDGE_LOOP('',(#7562,#7563,#7564,#7565,#7566,#7567,#7568,#7569,#7570,
#7571,#7572,#7573));
#2992=EDGE_LOOP('',(#7574,#7575,#7576,#7577,#7578,#7579,#7580,#7581,#7582,
#7583,#7584,#7585,#7586,#7587,#7588,#7589,#7590,#7591,#7592,#7593));
#2993=EDGE_LOOP('',(#7594,#7595,#7596,#7597,#7598,#7599,#7600,#7601,#7602,
#7603,#7604,#7605));
#2994=EDGE_LOOP('',(#7606,#7607,#7608,#7609,#7610,#7611,#7612,#7613,#7614,
#7615,#7616,#7617,#7618,#7619,#7620,#7621,#7622,#7623,#7624,#7625));
#2995=EDGE_LOOP('',(#7626,#7627,#7628,#7629,#7630,#7631,#7632,#7633,#7634,
#7635,#7636,#7637,#7638,#7639,#7640,#7641,#7642,#7643,#7644,#7645));
#2996=EDGE_LOOP('',(#7646,#7647,#7648,#7649,#7650,#7651,#7652,#7653,#7654,
#7655,#7656,#7657,#7658,#7659,#7660,#7661,#7662,#7663,#7664,#7665));
#2997=EDGE_LOOP('',(#7666,#7667,#7668,#7669));
#2998=EDGE_LOOP('',(#7670,#7671,#7672,#7673,#7674,#7675,#7676,#7677,#7678,
#7679,#7680,#7681));
#2999=EDGE_LOOP('',(#7682,#7683,#7684,#7685));
#3000=EDGE_LOOP('',(#7686,#7687,#7688,#7689));
#3001=EDGE_LOOP('',(#7690,#7691,#7692,#7693));
#3002=EDGE_LOOP('',(#7694,#7695,#7696,#7697));
#3003=EDGE_LOOP('',(#7698,#7699,#7700,#7701));
#3004=EDGE_LOOP('',(#7702,#7703,#7704,#7705));
#3005=EDGE_LOOP('',(#7706,#7707,#7708,#7709));
#3006=EDGE_LOOP('',(#7710,#7711,#7712,#7713));
#3007=EDGE_LOOP('',(#7714,#7715,#7716,#7717));
#3008=EDGE_LOOP('',(#7718,#7719,#7720,#7721));
#3009=EDGE_LOOP('',(#7722,#7723,#7724,#7725));
#3010=EDGE_LOOP('',(#7726,#7727,#7728,#7729));
#3011=EDGE_LOOP('',(#7730,#7731,#7732,#7733));
#3012=EDGE_LOOP('',(#7734,#7735,#7736,#7737));
#3013=EDGE_LOOP('',(#7738,#7739,#7740,#7741));
#3014=EDGE_LOOP('',(#7742,#7743,#7744,#7745));
#3015=EDGE_LOOP('',(#7746,#7747,#7748,#7749));
#3016=EDGE_LOOP('',(#7750,#7751,#7752,#7753));
#3017=EDGE_LOOP('',(#7754,#7755,#7756,#7757));
#3018=EDGE_LOOP('',(#7758,#7759,#7760,#7761));
#3019=EDGE_LOOP('',(#7762,#7763,#7764,#7765));
#3020=EDGE_LOOP('',(#7766,#7767,#7768,#7769));
#3021=EDGE_LOOP('',(#7770,#7771,#7772,#7773));
#3022=EDGE_LOOP('',(#7774,#7775,#7776,#7777));
#3023=EDGE_LOOP('',(#7778,#7779,#7780,#7781));
#3024=EDGE_LOOP('',(#7782,#7783,#7784,#7785));
#3025=EDGE_LOOP('',(#7786,#7787,#7788,#7789));
#3026=EDGE_LOOP('',(#7790,#7791,#7792,#7793));
#3027=EDGE_LOOP('',(#7794,#7795,#7796,#7797));
#3028=EDGE_LOOP('',(#7798,#7799,#7800,#7801));
#3029=EDGE_LOOP('',(#7802,#7803,#7804,#7805));
#3030=EDGE_LOOP('',(#7806,#7807,#7808,#7809));
#3031=EDGE_LOOP('',(#7810,#7811,#7812,#7813));
#3032=EDGE_LOOP('',(#7814,#7815,#7816,#7817));
#3033=EDGE_LOOP('',(#7818,#7819,#7820,#7821));
#3034=EDGE_LOOP('',(#7822,#7823,#7824,#7825));
#3035=EDGE_LOOP('',(#7826,#7827,#7828,#7829,#7830));
#3036=EDGE_LOOP('',(#7831,#7832,#7833,#7834));
#3037=EDGE_LOOP('',(#7835,#7836,#7837,#7838,#7839));
#3038=EDGE_LOOP('',(#7840,#7841,#7842,#7843,#7844));
#3039=EDGE_LOOP('',(#7845,#7846,#7847,#7848));
#3040=EDGE_LOOP('',(#7849,#7850,#7851,#7852));
#3041=EDGE_LOOP('',(#7853,#7854,#7855,#7856));
#3042=EDGE_LOOP('',(#7857,#7858,#7859,#7860));
#3043=EDGE_LOOP('',(#7861,#7862,#7863,#7864,#7865,#7866,#7867,#7868,#7869,
#7870,#7871,#7872,#7873,#7874,#7875,#7876));
#3044=EDGE_LOOP('',(#7877,#7878,#7879,#7880));
#3045=EDGE_LOOP('',(#7881,#7882,#7883,#7884));
#3046=EDGE_LOOP('',(#7885,#7886,#7887,#7888));
#3047=EDGE_LOOP('',(#7889,#7890,#7891,#7892));
#3048=EDGE_LOOP('',(#7893,#7894,#7895,#7896));
#3049=EDGE_LOOP('',(#7897,#7898,#7899,#7900));
#3050=EDGE_LOOP('',(#7901,#7902,#7903,#7904));
#3051=EDGE_LOOP('',(#7905,#7906,#7907,#7908));
#3052=EDGE_LOOP('',(#7909,#7910,#7911,#7912));
#3053=EDGE_LOOP('',(#7913,#7914,#7915,#7916));
#3054=EDGE_LOOP('',(#7917,#7918,#7919,#7920));
#3055=EDGE_LOOP('',(#7921,#7922,#7923,#7924));
#3056=EDGE_LOOP('',(#7925,#7926,#7927,#7928));
#3057=EDGE_LOOP('',(#7929,#7930,#7931,#7932,#7933,#7934,#7935,#7936,#7937,
#7938,#7939,#7940,#7941,#7942,#7943,#7944,#7945,#7946,#7947,#7948,#7949,
#7950,#7951,#7952));
#3058=EDGE_LOOP('',(#7953));
#3059=EDGE_LOOP('',(#7954));
#3060=EDGE_LOOP('',(#7955));
#3061=EDGE_LOOP('',(#7956,#7957,#7958,#7959,#7960,#7961,#7962,#7963,#7964,
#7965,#7966,#7967));
#3062=EDGE_LOOP('',(#7968));
#3063=EDGE_LOOP('',(#7969));
#3064=EDGE_LOOP('',(#7970));
#3065=EDGE_LOOP('',(#7971));
#3066=EDGE_LOOP('',(#7972));
#3067=EDGE_LOOP('',(#7973,#7974,#7975));
#3068=EDGE_LOOP('',(#7976,#7977,#7978));
#3069=EDGE_LOOP('',(#7979,#7980,#7981,#7982));
#3070=EDGE_LOOP('',(#7983,#7984,#7985,#7986));
#3071=EDGE_LOOP('',(#7987,#7988,#7989,#7990));
#3072=EDGE_LOOP('',(#7991,#7992,#7993,#7994));
#3073=EDGE_LOOP('',(#7995,#7996,#7997,#7998));
#3074=EDGE_LOOP('',(#7999,#8000,#8001,#8002));
#3075=EDGE_LOOP('',(#8003,#8004,#8005));
#3076=EDGE_LOOP('',(#8006,#8007,#8008,#8009));
#3077=EDGE_LOOP('',(#8010,#8011,#8012));
#3078=EDGE_LOOP('',(#8013,#8014,#8015,#8016));
#3079=EDGE_LOOP('',(#8017,#8018,#8019));
#3080=EDGE_LOOP('',(#8020,#8021,#8022));
#3081=EDGE_LOOP('',(#8023,#8024,#8025,#8026));
#3082=EDGE_LOOP('',(#8027,#8028,#8029));
#3083=EDGE_LOOP('',(#8030,#8031,#8032,#8033));
#3084=EDGE_LOOP('',(#8034,#8035,#8036));
#3085=EDGE_LOOP('',(#8037,#8038,#8039,#8040));
#3086=EDGE_LOOP('',(#8041,#8042,#8043));
#3087=EDGE_LOOP('',(#8044,#8045,#8046));
#3088=EDGE_LOOP('',(#8047,#8048,#8049,#8050));
#3089=EDGE_LOOP('',(#8051,#8052,#8053,#8054));
#3090=EDGE_LOOP('',(#8055,#8056,#8057,#8058));
#3091=EDGE_LOOP('',(#8059,#8060,#8061));
#3092=EDGE_LOOP('',(#8062,#8063,#8064,#8065));
#3093=EDGE_LOOP('',(#8066,#8067,#8068));
#3094=EDGE_LOOP('',(#8069,#8070,#8071));
#3095=EDGE_LOOP('',(#8072,#8073,#8074,#8075));
#3096=EDGE_LOOP('',(#8076,#8077,#8078));
#3097=EDGE_LOOP('',(#8079,#8080,#8081));
#3098=EDGE_LOOP('',(#8082,#8083,#8084));
#3099=EDGE_LOOP('',(#8085,#8086,#8087,#8088));
#3100=EDGE_LOOP('',(#8089,#8090,#8091,#8092));
#3101=EDGE_LOOP('',(#8093,#8094,#8095,#8096));
#3102=EDGE_LOOP('',(#8097,#8098,#8099,#8100));
#3103=EDGE_LOOP('',(#8101,#8102,#8103,#8104));
#3104=EDGE_LOOP('',(#8105,#8106,#8107,#8108));
#3105=EDGE_LOOP('',(#8109,#8110,#8111,#8112));
#3106=EDGE_LOOP('',(#8113,#8114,#8115,#8116));
#3107=EDGE_LOOP('',(#8117,#8118,#8119,#8120));
#3108=EDGE_LOOP('',(#8121,#8122,#8123,#8124));
#3109=EDGE_LOOP('',(#8125,#8126,#8127,#8128));
#3110=EDGE_LOOP('',(#8129,#8130,#8131,#8132));
#3111=EDGE_LOOP('',(#8133,#8134,#8135,#8136));
#3112=EDGE_LOOP('',(#8137,#8138,#8139,#8140));
#3113=EDGE_LOOP('',(#8141,#8142,#8143,#8144));
#3114=EDGE_LOOP('',(#8145,#8146,#8147,#8148));
#3115=EDGE_LOOP('',(#8149,#8150,#8151,#8152));
#3116=EDGE_LOOP('',(#8153,#8154,#8155,#8156));
#3117=EDGE_LOOP('',(#8157,#8158,#8159,#8160));
#3118=EDGE_LOOP('',(#8161,#8162,#8163,#8164));
#3119=EDGE_LOOP('',(#8165,#8166,#8167,#8168));
#3120=EDGE_LOOP('',(#8169,#8170,#8171,#8172));
#3121=EDGE_LOOP('',(#8173,#8174,#8175,#8176));
#3122=EDGE_LOOP('',(#8177,#8178,#8179,#8180));
#3123=EDGE_LOOP('',(#8181,#8182,#8183,#8184,#8185,#8186,#8187,#8188,#8189,
#8190,#8191,#8192,#8193,#8194,#8195,#8196));
#3124=EDGE_LOOP('',(#8197,#8198,#8199,#8200));
#3125=EDGE_LOOP('',(#8201,#8202,#8203,#8204));
#3126=EDGE_LOOP('',(#8205,#8206,#8207,#8208));
#3127=EDGE_LOOP('',(#8209,#8210,#8211,#8212));
#3128=EDGE_LOOP('',(#8213,#8214,#8215,#8216));
#3129=EDGE_LOOP('',(#8217));
#3130=EDGE_LOOP('',(#8218));
#3131=EDGE_LOOP('',(#8219));
#3132=EDGE_LOOP('',(#8220));
#3133=EDGE_LOOP('',(#8221));
#3134=EDGE_LOOP('',(#8222));
#3135=EDGE_LOOP('',(#8223));
#3136=EDGE_LOOP('',(#8224));
#3137=EDGE_LOOP('',(#8225));
#3138=EDGE_LOOP('',(#8226));
#3139=EDGE_LOOP('',(#8227));
#3140=EDGE_LOOP('',(#8228));
#3141=EDGE_LOOP('',(#8229));
#3142=EDGE_LOOP('',(#8230));
#3143=EDGE_LOOP('',(#8231));
#3144=EDGE_LOOP('',(#8232));
#3145=EDGE_LOOP('',(#8233));
#3146=EDGE_LOOP('',(#8234));
#3147=EDGE_LOOP('',(#8235));
#3148=EDGE_LOOP('',(#8236));
#3149=EDGE_LOOP('',(#8237));
#3150=EDGE_LOOP('',(#8238,#8239,#8240,#8241));
#3151=EDGE_LOOP('',(#8242,#8243,#8244,#8245,#8246));
#3152=EDGE_LOOP('',(#8247,#8248,#8249,#8250,#8251,#8252,#8253,#8254,#8255,
#8256,#8257,#8258,#8259,#8260,#8261,#8262));
#3153=EDGE_LOOP('',(#8263,#8264,#8265,#8266));
#3154=EDGE_LOOP('',(#8267,#8268,#8269,#8270));
#3155=EDGE_LOOP('',(#8271,#8272,#8273,#8274));
#3156=EDGE_LOOP('',(#8275,#8276,#8277,#8278));
#3157=EDGE_LOOP('',(#8279,#8280,#8281,#8282));
#3158=EDGE_LOOP('',(#8283,#8284,#8285,#8286));
#3159=EDGE_LOOP('',(#8287,#8288,#8289,#8290));
#3160=EDGE_LOOP('',(#8291,#8292,#8293,#8294));
#3161=EDGE_LOOP('',(#8295,#8296,#8297,#8298));
#3162=EDGE_LOOP('',(#8299,#8300,#8301));
#3163=EDGE_LOOP('',(#8302,#8303,#8304,#8305));
#3164=EDGE_LOOP('',(#8306,#8307,#8308,#8309));
#3165=EDGE_LOOP('',(#8310,#8311,#8312));
#3166=EDGE_LOOP('',(#8313,#8314,#8315));
#3167=EDGE_LOOP('',(#8316,#8317,#8318,#8319));
#3168=EDGE_LOOP('',(#8320,#8321,#8322));
#3169=EDGE_LOOP('',(#8323,#8324,#8325));
#3170=EDGE_LOOP('',(#8326,#8327,#8328));
#3171=EDGE_LOOP('',(#8329,#8330,#8331));
#3172=EDGE_LOOP('',(#8332,#8333,#8334,#8335));
#3173=EDGE_LOOP('',(#8336,#8337,#8338));
#3174=EDGE_LOOP('',(#8339,#8340,#8341,#8342));
#3175=EDGE_LOOP('',(#8343,#8344,#8345,#8346));
#3176=EDGE_LOOP('',(#8347,#8348,#8349,#8350));
#3177=EDGE_LOOP('',(#8351,#8352,#8353,#8354));
#3178=EDGE_LOOP('',(#8355,#8356,#8357,#8358));
#3179=EDGE_LOOP('',(#8359,#8360,#8361,#8362));
#3180=EDGE_LOOP('',(#8363,#8364,#8365,#8366));
#3181=EDGE_LOOP('',(#8367,#8368,#8369,#8370));
#3182=EDGE_LOOP('',(#8371,#8372,#8373,#8374));
#3183=EDGE_LOOP('',(#8375,#8376,#8377,#8378));
#3184=EDGE_LOOP('',(#8379,#8380,#8381,#8382));
#3185=EDGE_LOOP('',(#8383,#8384,#8385,#8386));
#3186=EDGE_LOOP('',(#8387,#8388,#8389,#8390));
#3187=EDGE_LOOP('',(#8391,#8392,#8393,#8394));
#3188=EDGE_LOOP('',(#8395,#8396,#8397,#8398));
#3189=EDGE_LOOP('',(#8399,#8400,#8401,#8402,#8403,#8404,#8405));
#3190=EDGE_LOOP('',(#8406,#8407,#8408,#8409));
#3191=EDGE_LOOP('',(#8410,#8411,#8412,#8413));
#3192=EDGE_LOOP('',(#8414,#8415,#8416,#8417));
#3193=EDGE_LOOP('',(#8418,#8419,#8420,#8421));
#3194=EDGE_LOOP('',(#8422,#8423,#8424,#8425,#8426,#8427,#8428));
#3195=EDGE_LOOP('',(#8429,#8430,#8431,#8432));
#3196=EDGE_LOOP('',(#8433,#8434,#8435,#8436));
#3197=EDGE_LOOP('',(#8437,#8438,#8439,#8440));
#3198=EDGE_LOOP('',(#8441,#8442,#8443,#8444));
#3199=EDGE_LOOP('',(#8445,#8446,#8447,#8448));
#3200=EDGE_LOOP('',(#8449,#8450,#8451,#8452));
#3201=EDGE_LOOP('',(#8453,#8454,#8455,#8456));
#3202=EDGE_LOOP('',(#8457));
#3203=EDGE_LOOP('',(#8458));
#3204=EDGE_LOOP('',(#8459,#8460,#8461,#8462));
#3205=EDGE_LOOP('',(#8463,#8464,#8465,#8466));
#3206=EDGE_LOOP('',(#8467));
#3207=EDGE_LOOP('',(#8468,#8469,#8470,#8471));
#3208=EDGE_LOOP('',(#8472,#8473,#8474,#8475));
#3209=EDGE_LOOP('',(#8476));
#3210=EDGE_LOOP('',(#8477,#8478,#8479,#8480));
#3211=EDGE_LOOP('',(#8481,#8482,#8483,#8484));
#3212=EDGE_LOOP('',(#8485,#8486,#8487,#8488));
#3213=EDGE_LOOP('',(#8489,#8490,#8491,#8492));
#3214=EDGE_LOOP('',(#8493,#8494,#8495,#8496));
#3215=EDGE_LOOP('',(#8497,#8498,#8499,#8500));
#3216=EDGE_LOOP('',(#8501,#8502,#8503,#8504));
#3217=EDGE_LOOP('',(#8505,#8506,#8507,#8508));
#3218=EDGE_LOOP('',(#8509,#8510,#8511,#8512));
#3219=EDGE_LOOP('',(#8513,#8514,#8515));
#3220=EDGE_LOOP('',(#8516,#8517,#8518,#8519));
#3221=EDGE_LOOP('',(#8520,#8521,#8522,#8523));
#3222=EDGE_LOOP('',(#8524,#8525,#8526));
#3223=EDGE_LOOP('',(#8527,#8528,#8529));
#3224=EDGE_LOOP('',(#8530,#8531,#8532,#8533));
#3225=EDGE_LOOP('',(#8534,#8535,#8536));
#3226=EDGE_LOOP('',(#8537,#8538,#8539));
#3227=EDGE_LOOP('',(#8540,#8541,#8542));
#3228=EDGE_LOOP('',(#8543,#8544,#8545));
#3229=EDGE_LOOP('',(#8546,#8547,#8548,#8549));
#3230=EDGE_LOOP('',(#8550,#8551,#8552));
#3231=EDGE_LOOP('',(#8553,#8554,#8555,#8556));
#3232=EDGE_LOOP('',(#8557,#8558,#8559,#8560));
#3233=EDGE_LOOP('',(#8561,#8562,#8563,#8564));
#3234=EDGE_LOOP('',(#8565,#8566,#8567,#8568));
#3235=EDGE_LOOP('',(#8569,#8570,#8571,#8572));
#3236=EDGE_LOOP('',(#8573,#8574,#8575,#8576));
#3237=EDGE_LOOP('',(#8577,#8578,#8579,#8580));
#3238=EDGE_LOOP('',(#8581,#8582,#8583,#8584));
#3239=EDGE_LOOP('',(#8585,#8586,#8587,#8588));
#3240=EDGE_LOOP('',(#8589,#8590,#8591,#8592));
#3241=EDGE_LOOP('',(#8593,#8594,#8595,#8596));
#3242=EDGE_LOOP('',(#8597,#8598,#8599,#8600));
#3243=EDGE_LOOP('',(#8601,#8602,#8603,#8604));
#3244=EDGE_LOOP('',(#8605,#8606,#8607,#8608));
#3245=EDGE_LOOP('',(#8609,#8610,#8611,#8612));
#3246=EDGE_LOOP('',(#8613,#8614,#8615,#8616,#8617,#8618,#8619));
#3247=EDGE_LOOP('',(#8620,#8621,#8622,#8623));
#3248=EDGE_LOOP('',(#8624,#8625,#8626,#8627));
#3249=EDGE_LOOP('',(#8628,#8629,#8630,#8631));
#3250=EDGE_LOOP('',(#8632,#8633,#8634,#8635));
#3251=EDGE_LOOP('',(#8636,#8637,#8638,#8639,#8640,#8641,#8642));
#3252=EDGE_LOOP('',(#8643,#8644,#8645,#8646));
#3253=EDGE_LOOP('',(#8647,#8648,#8649,#8650));
#3254=EDGE_LOOP('',(#8651,#8652,#8653,#8654));
#3255=EDGE_LOOP('',(#8655,#8656,#8657,#8658));
#3256=EDGE_LOOP('',(#8659,#8660,#8661,#8662));
#3257=EDGE_LOOP('',(#8663,#8664,#8665,#8666));
#3258=EDGE_LOOP('',(#8667,#8668,#8669,#8670));
#3259=EDGE_LOOP('',(#8671,#8672,#8673,#8674));
#3260=EDGE_LOOP('',(#8675,#8676,#8677,#8678));
#3261=EDGE_LOOP('',(#8679,#8680,#8681,#8682));
#3262=EDGE_LOOP('',(#8683,#8684,#8685,#8686));
#3263=EDGE_LOOP('',(#8687,#8688,#8689,#8690));
#3264=EDGE_LOOP('',(#8691,#8692,#8693,#8694));
#3265=EDGE_LOOP('',(#8695,#8696,#8697,#8698));
#3266=EDGE_LOOP('',(#8699,#8700,#8701,#8702));
#3267=EDGE_LOOP('',(#8703,#8704,#8705,#8706));
#3268=EDGE_LOOP('',(#8707,#8708,#8709));
#3269=EDGE_LOOP('',(#8710,#8711,#8712,#8713));
#3270=EDGE_LOOP('',(#8714,#8715,#8716,#8717));
#3271=EDGE_LOOP('',(#8718,#8719,#8720));
#3272=EDGE_LOOP('',(#8721,#8722,#8723));
#3273=EDGE_LOOP('',(#8724,#8725,#8726,#8727));
#3274=EDGE_LOOP('',(#8728,#8729,#8730));
#3275=EDGE_LOOP('',(#8731,#8732,#8733));
#3276=EDGE_LOOP('',(#8734,#8735,#8736));
#3277=EDGE_LOOP('',(#8737,#8738,#8739));
#3278=EDGE_LOOP('',(#8740,#8741,#8742,#8743));
#3279=EDGE_LOOP('',(#8744,#8745,#8746));
#3280=EDGE_LOOP('',(#8747,#8748,#8749,#8750));
#3281=EDGE_LOOP('',(#8751,#8752,#8753,#8754));
#3282=EDGE_LOOP('',(#8755,#8756,#8757,#8758));
#3283=EDGE_LOOP('',(#8759,#8760,#8761,#8762));
#3284=EDGE_LOOP('',(#8763,#8764,#8765,#8766));
#3285=EDGE_LOOP('',(#8767,#8768,#8769,#8770));
#3286=EDGE_LOOP('',(#8771,#8772,#8773,#8774));
#3287=EDGE_LOOP('',(#8775,#8776,#8777,#8778));
#3288=EDGE_LOOP('',(#8779,#8780,#8781,#8782));
#3289=EDGE_LOOP('',(#8783,#8784,#8785,#8786));
#3290=EDGE_LOOP('',(#8787,#8788,#8789,#8790));
#3291=EDGE_LOOP('',(#8791,#8792,#8793,#8794));
#3292=EDGE_LOOP('',(#8795,#8796,#8797,#8798));
#3293=EDGE_LOOP('',(#8799,#8800,#8801,#8802));
#3294=EDGE_LOOP('',(#8803,#8804,#8805,#8806));
#3295=EDGE_LOOP('',(#8807,#8808,#8809,#8810,#8811,#8812,#8813));
#3296=EDGE_LOOP('',(#8814,#8815,#8816,#8817));
#3297=EDGE_LOOP('',(#8818,#8819,#8820,#8821));
#3298=EDGE_LOOP('',(#8822,#8823,#8824,#8825));
#3299=EDGE_LOOP('',(#8826,#8827,#8828,#8829));
#3300=EDGE_LOOP('',(#8830,#8831,#8832,#8833,#8834,#8835,#8836));
#3301=EDGE_LOOP('',(#8837,#8838,#8839,#8840));
#3302=EDGE_LOOP('',(#8841,#8842,#8843,#8844));
#3303=EDGE_LOOP('',(#8845,#8846,#8847,#8848));
#3304=EDGE_LOOP('',(#8849,#8850,#8851,#8852));
#3305=EDGE_LOOP('',(#8853,#8854,#8855,#8856));
#3306=EDGE_LOOP('',(#8857,#8858,#8859,#8860));
#3307=EDGE_LOOP('',(#8861,#8862,#8863,#8864));
#3308=CIRCLE('',#9752,8.);
#3309=CIRCLE('',#9753,7.5);
#3310=CIRCLE('',#9755,8.);
#3311=CIRCLE('',#9756,9.);
#3312=CIRCLE('',#9758,9.);
#3313=CIRCLE('',#9762,7.5);
#3314=CIRCLE('',#9766,0.5);
#3315=CIRCLE('',#9767,0.5);
#3316=CIRCLE('',#9769,0.5);
#3317=CIRCLE('',#9770,0.5);
#3318=CIRCLE('',#9775,0.500000000000007);
#3319=CIRCLE('',#9781,0.500000000000007);
#3320=CIRCLE('',#9783,0.999999999999972);
#3321=CIRCLE('',#9784,1.);
#3322=CIRCLE('',#9785,0.999999999999997);
#3323=CIRCLE('',#9786,0.999999999999996);
#3324=CIRCLE('',#9788,0.5);
#3325=CIRCLE('',#9789,0.5);
#3326=CIRCLE('',#9791,0.5);
#3327=CIRCLE('',#9792,0.5);
#3328=CIRCLE('',#9795,0.500000000000007);
#3329=CIRCLE('',#9797,1.);
#3330=CIRCLE('',#9798,1.);
#3331=CIRCLE('',#9799,1.);
#3332=CIRCLE('',#9800,0.999999999999992);
#3333=CIRCLE('',#9803,0.500000000000007);
#3334=CIRCLE('',#9805,0.5);
#3335=CIRCLE('',#9806,0.499999999999998);
#3336=CIRCLE('',#9807,0.500000000000007);
#3337=CIRCLE('',#9809,0.500000000000007);
#3338=CIRCLE('',#9810,0.5);
#3339=CIRCLE('',#9811,0.500000000000007);
#3340=CIRCLE('',#9813,0.500000000000007);
#3341=CIRCLE('',#9814,0.499999999999998);
#3342=CIRCLE('',#9815,0.5);
#3343=CIRCLE('',#9817,0.500000000000007);
#3344=CIRCLE('',#9818,0.499999999999998);
#3345=CIRCLE('',#9819,0.499999999999998);
#3346=CIRCLE('',#9822,0.500000000000007);
#3347=CIRCLE('',#9823,0.5);
#3348=CIRCLE('',#9824,0.499999999999998);
#3349=CIRCLE('',#9828,0.5);
#3350=CIRCLE('',#9829,0.499999999999998);
#3351=CIRCLE('',#9830,0.500000000000007);
#3352=CIRCLE('',#9834,0.5);
#3353=CIRCLE('',#9835,0.499999999999998);
#3354=CIRCLE('',#9836,0.500000000000007);
#3355=CIRCLE('',#9838,0.499999999999998);
#3356=CIRCLE('',#9839,0.5);
#3357=CIRCLE('',#9841,0.499999999999998);
#3358=CIRCLE('',#9842,0.5);
#3359=CIRCLE('',#9843,0.500000000000007);
#3360=CIRCLE('',#9847,0.500000000000007);
#3361=CIRCLE('',#9848,0.5);
#3362=CIRCLE('',#9850,0.500000000000005);
#3363=CIRCLE('',#9851,0.5);
#3364=CIRCLE('',#9852,0.500000000000007);
#3365=CIRCLE('',#9854,0.5);
#3366=CIRCLE('',#9855,0.5);
#3367=CIRCLE('',#9856,0.500000000000007);
#3368=CIRCLE('',#9860,0.500000000000007);
#3369=CIRCLE('',#9861,0.5);
#3370=CIRCLE('',#9862,0.499999999999998);
#3371=CIRCLE('',#9864,0.500000000000007);
#3372=CIRCLE('',#9865,0.5);
#3373=CIRCLE('',#9866,0.499999999999998);
#3374=CIRCLE('',#9869,0.500000000000007);
#3375=CIRCLE('',#9870,0.5);
#3376=CIRCLE('',#9871,0.5);
#3377=CIRCLE('',#9875,0.5);
#3378=CIRCLE('',#9876,0.500000000000007);
#3379=CIRCLE('',#9880,0.499999999999999);
#3380=CIRCLE('',#9881,0.499999999999998);
#3381=CIRCLE('',#9882,0.500000000000007);
#3382=CIRCLE('',#9884,0.500000000000007);
#3383=CIRCLE('',#9885,0.5);
#3384=CIRCLE('',#9888,0.5);
#3385=CIRCLE('',#9889,0.499999999999999);
#3386=CIRCLE('',#9890,0.500000000000007);
#3387=CIRCLE('',#9892,0.499999999999998);
#3388=CIRCLE('',#9893,0.500000000000007);
#3389=CIRCLE('',#9894,0.5);
#3390=CIRCLE('',#9897,0.499999999999999);
#3391=CIRCLE('',#9898,0.500000000000007);
#3392=CIRCLE('',#9899,0.5);
#3393=CIRCLE('',#9903,0.499999999999999);
#3394=CIRCLE('',#9904,0.499999999999998);
#3395=CIRCLE('',#9905,0.500000000000007);
#3396=CIRCLE('',#9934,6.);
#3397=CIRCLE('',#9935,6.);
#3398=CIRCLE('',#9937,6.);
#3399=CIRCLE('',#9938,6.);
#3400=CIRCLE('',#9941,6.);
#3401=CIRCLE('',#9942,6.);
#3402=CIRCLE('',#9945,6.);
#3403=CIRCLE('',#9946,6.);
#3404=CIRCLE('',#9948,0.499999999999999);
#3405=CIRCLE('',#9949,0.500000000000025);
#3406=CIRCLE('',#9950,0.499999999999998);
#3407=CIRCLE('',#9952,0.500000000000007);
#3408=CIRCLE('',#9953,0.500000000000005);
#3409=CIRCLE('',#9954,0.5);
#3410=CIRCLE('',#9956,0.499999999999998);
#3411=CIRCLE('',#9957,0.500000000000007);
#3412=CIRCLE('',#9958,0.999999999999996);
#3413=CIRCLE('',#9959,0.5);
#3414=CIRCLE('',#9962,1.);
#3415=CIRCLE('',#9963,0.500000000000002);
#3416=CIRCLE('',#9964,0.499999999999998);
#3417=CIRCLE('',#9965,0.500000000000007);
#3418=CIRCLE('',#9967,0.5);
#3419=CIRCLE('',#9968,0.500000000000007);
#3420=CIRCLE('',#9969,1.);
#3421=CIRCLE('',#9970,0.499999999999998);
#3422=CIRCLE('',#9972,1.00000000000001);
#3423=CIRCLE('',#9973,0.499999999999998);
#3424=CIRCLE('',#9974,0.499999999999999);
#3425=CIRCLE('',#9975,0.500000000000007);
#3426=CIRCLE('',#9978,0.5);
#3427=CIRCLE('',#9979,0.500000000000007);
#3428=CIRCLE('',#9980,0.499999999999999);
#3429=CIRCLE('',#9983,0.500000000000007);
#3430=CIRCLE('',#9984,0.499999999999998);
#3431=CIRCLE('',#9985,0.499999999999998);
#3432=CIRCLE('',#9988,0.499999999999999);
#3433=CIRCLE('',#9989,0.500000000000007);
#3434=CIRCLE('',#9990,0.5);
#3435=CIRCLE('',#9992,0.499999999999998);
#3436=CIRCLE('',#9993,0.500000000000007);
#3437=CIRCLE('',#9994,0.500000000000007);
#3438=CIRCLE('',#9997,0.5);
#3439=CIRCLE('',#9998,0.500000000000007);
#3440=CIRCLE('',#9999,0.499999999999998);
#3441=CIRCLE('',#10002,0.500000000000007);
#3442=CIRCLE('',#10003,0.500000000000007);
#3443=CIRCLE('',#10004,0.499999999999998);
#3444=CIRCLE('',#10007,0.499999999999998);
#3445=CIRCLE('',#10008,0.500000000000007);
#3446=CIRCLE('',#10009,0.499999999999999);
#3447=CIRCLE('',#10011,0.499999999999998);
#3448=CIRCLE('',#10012,0.500000000000007);
#3449=CIRCLE('',#10013,0.499999999999998);
#3450=CIRCLE('',#10016,0.499999999999998);
#3451=CIRCLE('',#10017,0.500000000000007);
#3452=CIRCLE('',#10018,0.999999999999996);
#3453=CIRCLE('',#10019,0.499999999999998);
#3454=CIRCLE('',#10022,0.499999999999998);
#3455=CIRCLE('',#10023,0.500000000000007);
#3456=CIRCLE('',#10024,0.499999999999998);
#3457=CIRCLE('',#10026,0.5);
#3458=CIRCLE('',#10027,0.500000000000007);
#3459=CIRCLE('',#10028,0.999999999999999);
#3460=CIRCLE('',#10029,0.499999999999998);
#3461=CIRCLE('',#10031,0.500000000000007);
#3462=CIRCLE('',#10032,0.500000000000007);
#3463=CIRCLE('',#10033,0.499999999999998);
#3464=CIRCLE('',#10035,0.499999999999998);
#3465=CIRCLE('',#10036,0.500000000000007);
#3466=CIRCLE('',#10037,0.500000000000007);
#3467=CIRCLE('',#10040,0.500000000000007);
#3468=CIRCLE('',#10041,0.499999999999998);
#3469=CIRCLE('',#10042,0.500000000000007);
#3470=CIRCLE('',#10044,0.499999999999998);
#3471=CIRCLE('',#10045,0.500000000000007);
#3472=CIRCLE('',#10046,0.499999999999998);
#3473=CIRCLE('',#10048,0.500000000000007);
#3474=CIRCLE('',#10049,0.499999999999998);
#3475=CIRCLE('',#10050,0.499999999999998);
#3476=CIRCLE('',#10052,0.499999999999998);
#3477=CIRCLE('',#10053,0.500000000000007);
#3478=CIRCLE('',#10054,1.00000000000001);
#3479=CIRCLE('',#10055,0.499999999999998);
#3480=CIRCLE('',#10059,0.499999999999998);
#3481=CIRCLE('',#10060,0.500000000000007);
#3482=CIRCLE('',#10061,0.999999999999996);
#3483=CIRCLE('',#10062,0.500000000000007);
#3484=CIRCLE('',#10103,4.);
#3485=CIRCLE('',#10104,4.);
#3486=CIRCLE('',#10107,4.);
#3487=CIRCLE('',#10108,4.);
#3488=CIRCLE('',#10111,4.);
#3489=CIRCLE('',#10112,4.);
#3490=CIRCLE('',#10115,4.);
#3491=CIRCLE('',#10116,4.);
#3492=CIRCLE('',#10119,4.);
#3493=CIRCLE('',#10120,4.);
#3494=CIRCLE('',#10123,4.);
#3495=CIRCLE('',#10124,4.);
#3496=CIRCLE('',#10127,4.);
#3497=CIRCLE('',#10128,4.);
#3498=CIRCLE('',#10131,4.);
#3499=CIRCLE('',#10132,4.);
#3500=CIRCLE('',#10135,0.5);
#3501=CIRCLE('',#10136,0.5);
#3502=CIRCLE('',#10138,0.5);
#3503=CIRCLE('',#10139,0.5);
#3504=CIRCLE('',#10144,0.500000000000007);
#3505=CIRCLE('',#10150,0.500000000000007);
#3506=CIRCLE('',#10152,0.999999999999972);
#3507=CIRCLE('',#10153,1.);
#3508=CIRCLE('',#10154,0.999999999999997);
#3509=CIRCLE('',#10155,0.999999999999996);
#3510=CIRCLE('',#10157,0.5);
#3511=CIRCLE('',#10158,0.5);
#3512=CIRCLE('',#10160,0.5);
#3513=CIRCLE('',#10161,0.5);
#3514=CIRCLE('',#10164,0.500000000000007);
#3515=CIRCLE('',#10166,1.);
#3516=CIRCLE('',#10167,1.);
#3517=CIRCLE('',#10168,1.);
#3518=CIRCLE('',#10169,0.999999999999992);
#3519=CIRCLE('',#10172,0.500000000000007);
#3520=CIRCLE('',#10174,0.5);
#3521=CIRCLE('',#10175,0.499999999999998);
#3522=CIRCLE('',#10176,0.500000000000007);
#3523=CIRCLE('',#10178,0.500000000000007);
#3524=CIRCLE('',#10179,0.5);
#3525=CIRCLE('',#10180,0.500000000000007);
#3526=CIRCLE('',#10182,0.500000000000007);
#3527=CIRCLE('',#10183,0.499999999999998);
#3528=CIRCLE('',#10184,0.5);
#3529=CIRCLE('',#10186,0.500000000000007);
#3530=CIRCLE('',#10187,0.499999999999998);
#3531=CIRCLE('',#10188,0.499999999999998);
#3532=CIRCLE('',#10191,0.500000000000007);
#3533=CIRCLE('',#10192,0.5);
#3534=CIRCLE('',#10193,0.499999999999998);
#3535=CIRCLE('',#10197,0.5);
#3536=CIRCLE('',#10198,0.499999999999998);
#3537=CIRCLE('',#10199,0.500000000000007);
#3538=CIRCLE('',#10203,0.5);
#3539=CIRCLE('',#10204,0.499999999999998);
#3540=CIRCLE('',#10205,0.500000000000007);
#3541=CIRCLE('',#10207,0.499999999999998);
#3542=CIRCLE('',#10208,0.5);
#3543=CIRCLE('',#10210,0.499999999999998);
#3544=CIRCLE('',#10211,0.5);
#3545=CIRCLE('',#10212,0.500000000000007);
#3546=CIRCLE('',#10216,0.500000000000007);
#3547=CIRCLE('',#10217,0.5);
#3548=CIRCLE('',#10219,0.500000000000005);
#3549=CIRCLE('',#10220,0.5);
#3550=CIRCLE('',#10221,0.500000000000007);
#3551=CIRCLE('',#10223,0.5);
#3552=CIRCLE('',#10224,0.5);
#3553=CIRCLE('',#10225,0.500000000000007);
#3554=CIRCLE('',#10229,0.500000000000007);
#3555=CIRCLE('',#10230,0.5);
#3556=CIRCLE('',#10231,0.499999999999998);
#3557=CIRCLE('',#10233,0.500000000000007);
#3558=CIRCLE('',#10234,0.5);
#3559=CIRCLE('',#10235,0.499999999999998);
#3560=CIRCLE('',#10238,0.500000000000007);
#3561=CIRCLE('',#10239,0.5);
#3562=CIRCLE('',#10240,0.5);
#3563=CIRCLE('',#10244,0.5);
#3564=CIRCLE('',#10245,0.500000000000007);
#3565=CIRCLE('',#10249,0.499999999999999);
#3566=CIRCLE('',#10250,0.499999999999998);
#3567=CIRCLE('',#10251,0.500000000000007);
#3568=CIRCLE('',#10253,0.500000000000007);
#3569=CIRCLE('',#10254,0.5);
#3570=CIRCLE('',#10257,0.5);
#3571=CIRCLE('',#10258,0.499999999999999);
#3572=CIRCLE('',#10259,0.500000000000007);
#3573=CIRCLE('',#10261,0.499999999999998);
#3574=CIRCLE('',#10262,0.500000000000007);
#3575=CIRCLE('',#10263,0.5);
#3576=CIRCLE('',#10266,0.499999999999999);
#3577=CIRCLE('',#10267,0.500000000000007);
#3578=CIRCLE('',#10268,0.5);
#3579=CIRCLE('',#10272,0.499999999999999);
#3580=CIRCLE('',#10273,0.499999999999998);
#3581=CIRCLE('',#10274,0.500000000000007);
#3582=CIRCLE('',#10303,0.3);
#3583=CIRCLE('',#10304,0.299999999999994);
#3584=CIRCLE('',#10306,0.300000000000011);
#3585=CIRCLE('',#10307,4.49999999999999);
#3586=CIRCLE('',#10308,4.79999999999999);
#3587=CIRCLE('',#10310,0.300000000000002);
#3588=CIRCLE('',#10312,4.49999999999998);
#3589=CIRCLE('',#10313,4.79999999999998);
#3590=CIRCLE('',#10315,4.49999999999999);
#3591=CIRCLE('',#10319,0.3);
#3592=CIRCLE('',#10320,0.599999999999987);
#3593=CIRCLE('',#10321,0.300000000000011);
#3594=CIRCLE('',#10322,0.299999999999994);
#3595=CIRCLE('',#10324,0.3);
#3596=CIRCLE('',#10325,0.300000000000011);
#3597=CIRCLE('',#10326,0.299999999999994);
#3598=CIRCLE('',#10328,0.600000000000001);
#3599=CIRCLE('',#10329,0.300000000000011);
#3600=CIRCLE('',#10330,0.3);
#3601=CIRCLE('',#10331,0.299999999999976);
#3602=CIRCLE('',#10335,0.300000000000003);
#3603=CIRCLE('',#10336,0.300000000000011);
#3604=CIRCLE('',#10337,0.3);
#3605=CIRCLE('',#10339,0.3);
#3606=CIRCLE('',#10340,0.300000000000011);
#3607=CIRCLE('',#10341,0.299999999999994);
#3608=CIRCLE('',#10344,0.299999999999994);
#3609=CIRCLE('',#10345,0.300000000000011);
#3610=CIRCLE('',#10346,0.3);
#3611=CIRCLE('',#10348,0.300000000000006);
#3612=CIRCLE('',#10349,0.3);
#3613=CIRCLE('',#10350,0.300000000000011);
#3614=CIRCLE('',#10352,0.3);
#3615=CIRCLE('',#10353,0.300000000000011);
#3616=CIRCLE('',#10354,0.300000000000003);
#3617=CIRCLE('',#10356,0.300000000000011);
#3618=CIRCLE('',#10357,0.3);
#3619=CIRCLE('',#10358,0.299999999999994);
#3620=CIRCLE('',#10361,0.3);
#3621=CIRCLE('',#10362,0.300000000000001);
#3622=CIRCLE('',#10363,0.300000000000011);
#3623=CIRCLE('',#10383,4.79999999999999);
#3624=CIRCLE('',#10384,4.79999999999998);
#3625=CIRCLE('',#10388,0.3);
#3626=CIRCLE('',#10389,0.299999999999994);
#3627=CIRCLE('',#10391,0.300000000000002);
#3628=CIRCLE('',#10392,4.49999999999998);
#3629=CIRCLE('',#10394,0.300000000000002);
#3630=CIRCLE('',#10401,12.5);
#3631=CIRCLE('',#10402,12.5);
#3632=CIRCLE('',#10404,12.5);
#3633=CIRCLE('',#10405,12.5);
#3634=CIRCLE('',#10406,12.5);
#3635=CIRCLE('',#10407,12.5);
#3636=CIRCLE('',#10409,5.);
#3637=CIRCLE('',#10410,5.);
#3638=CIRCLE('',#10411,5.);
#3639=CIRCLE('',#10412,5.);
#3640=CIRCLE('',#10413,12.5);
#3641=CIRCLE('',#10414,5.);
#3642=CIRCLE('',#10415,5.);
#3643=CIRCLE('',#10416,5.);
#3644=CIRCLE('',#10417,5.);
#3645=CIRCLE('',#10418,5.);
#3646=CIRCLE('',#10419,5.);
#3647=CIRCLE('',#10421,0.499999999999998);
#3648=CIRCLE('',#10424,0.499999999999998);
#3649=CIRCLE('',#10426,5.);
#3650=CIRCLE('',#10427,5.);
#3651=CIRCLE('',#10429,5.);
#3652=CIRCLE('',#10430,5.);
#3653=CIRCLE('',#10432,5.);
#3654=CIRCLE('',#10433,5.);
#3655=CIRCLE('',#10435,5.);
#3656=CIRCLE('',#10436,5.);
#3657=CIRCLE('',#10437,5.);
#3658=CIRCLE('',#10439,12.5);
#3659=CIRCLE('',#10440,12.5);
#3660=CIRCLE('',#10442,5.);
#3661=CIRCLE('',#10443,5.);
#3662=CIRCLE('',#10444,5.);
#3663=CIRCLE('',#10446,5.);
#3664=CIRCLE('',#10447,5.);
#3665=CIRCLE('',#10449,5.);
#3666=CIRCLE('',#10450,5.);
#3667=CIRCLE('',#10451,5.);
#3668=CIRCLE('',#10453,5.);
#3669=CIRCLE('',#10454,5.);
#3670=CIRCLE('',#10456,5.);
#3671=CIRCLE('',#10457,5.);
#3672=CIRCLE('',#10459,5.);
#3673=CIRCLE('',#10460,5.);
#3674=CIRCLE('',#10462,5.);
#3675=CIRCLE('',#10463,5.);
#3676=CIRCLE('',#10464,5.);
#3677=CIRCLE('',#10466,5.);
#3678=CIRCLE('',#10467,5.);
#3679=CIRCLE('',#10468,5.);
#3680=CIRCLE('',#10469,5.);
#3681=CIRCLE('',#10471,5.);
#3682=CIRCLE('',#10473,5.);
#3683=CIRCLE('',#10475,12.5);
#3684=CIRCLE('',#10476,12.5);
#3685=CIRCLE('',#10477,12.5);
#3686=CIRCLE('',#10479,5.);
#3687=CIRCLE('',#10480,5.);
#3688=CIRCLE('',#10481,5.);
#3689=CIRCLE('',#10482,5.);
#3690=CIRCLE('',#10484,5.);
#3691=CIRCLE('',#10486,5.);
#3692=CIRCLE('',#10488,5.);
#3693=CIRCLE('',#10489,5.);
#3694=CIRCLE('',#10490,5.);
#3695=CIRCLE('',#10491,5.);
#3696=CIRCLE('',#10493,5.);
#3697=CIRCLE('',#10495,5.);
#3698=CIRCLE('',#10497,5.);
#3699=CIRCLE('',#10498,5.);
#3700=CIRCLE('',#10499,5.);
#3701=CIRCLE('',#10500,5.);
#3702=CIRCLE('',#10502,5.);
#3703=CIRCLE('',#10504,5.);
#3704=CIRCLE('',#10506,5.);
#3705=CIRCLE('',#10507,5.);
#3706=CIRCLE('',#10509,5.);
#3707=CIRCLE('',#10510,5.);
#3708=CIRCLE('',#10513,0.5);
#3709=CIRCLE('',#10516,0.499999999999998);
#3710=CIRCLE('',#10524,0.499999999999998);
#3711=CIRCLE('',#10527,0.5);
#3712=CIRCLE('',#10529,0.499999999999999);
#3713=CIRCLE('',#10532,0.5);
#3714=CIRCLE('',#10541,0.499999999999999);
#3715=CIRCLE('',#10544,0.499999999999998);
#3716=CIRCLE('',#10547,0.5);
#3717=CIRCLE('',#10550,0.499999999999998);
#3718=CIRCLE('',#10562,0.5);
#3719=CIRCLE('',#10565,0.499999999999999);
#3720=CIRCLE('',#10570,0.499999999999998);
#3721=CIRCLE('',#10580,0.499999999999998);
#3722=CIRCLE('',#10586,0.500000000000025);
#3723=CIRCLE('',#10587,0.499999999999998);
#3724=CIRCLE('',#10589,0.500000000000007);
#3725=CIRCLE('',#10590,0.500000000000005);
#3726=CIRCLE('',#10592,0.500000000000007);
#3727=CIRCLE('',#10593,0.999999999999996);
#3728=CIRCLE('',#10594,0.5);
#3729=CIRCLE('',#10597,1.);
#3730=CIRCLE('',#10598,0.500000000000002);
#3731=CIRCLE('',#10599,0.500000000000007);
#3732=CIRCLE('',#10601,0.500000000000007);
#3733=CIRCLE('',#10602,1.);
#3734=CIRCLE('',#10603,0.499999999999998);
#3735=CIRCLE('',#10605,1.00000000000001);
#3736=CIRCLE('',#10606,0.499999999999998);
#3737=CIRCLE('',#10607,0.500000000000007);
#3738=CIRCLE('',#10610,0.500000000000007);
#3739=CIRCLE('',#10611,0.499999999999999);
#3740=CIRCLE('',#10614,0.500000000000007);
#3741=CIRCLE('',#10615,0.499999999999998);
#3742=CIRCLE('',#10616,0.499999999999998);
#3743=CIRCLE('',#10619,0.500000000000007);
#3744=CIRCLE('',#10620,0.5);
#3745=CIRCLE('',#10622,0.499999999999998);
#3746=CIRCLE('',#10623,0.500000000000007);
#3747=CIRCLE('',#10624,0.500000000000007);
#3748=CIRCLE('',#10627,0.500000000000007);
#3749=CIRCLE('',#10628,0.499999999999998);
#3750=CIRCLE('',#10631,0.500000000000007);
#3751=CIRCLE('',#10632,0.500000000000007);
#3752=CIRCLE('',#10633,0.499999999999998);
#3753=CIRCLE('',#10636,0.500000000000007);
#3754=CIRCLE('',#10637,0.499999999999999);
#3755=CIRCLE('',#10639,0.499999999999998);
#3756=CIRCLE('',#10640,0.500000000000007);
#3757=CIRCLE('',#10641,0.499999999999998);
#3758=CIRCLE('',#10644,0.500000000000007);
#3759=CIRCLE('',#10645,0.999999999999996);
#3760=CIRCLE('',#10646,0.499999999999998);
#3761=CIRCLE('',#10649,0.499999999999998);
#3762=CIRCLE('',#10650,0.500000000000007);
#3763=CIRCLE('',#10651,0.499999999999998);
#3764=CIRCLE('',#10653,0.500000000000007);
#3765=CIRCLE('',#10654,0.999999999999999);
#3766=CIRCLE('',#10655,0.499999999999998);
#3767=CIRCLE('',#10657,0.500000000000007);
#3768=CIRCLE('',#10658,0.500000000000007);
#3769=CIRCLE('',#10659,0.499999999999998);
#3770=CIRCLE('',#10661,0.500000000000007);
#3771=CIRCLE('',#10662,0.500000000000007);
#3772=CIRCLE('',#10665,0.500000000000007);
#3773=CIRCLE('',#10666,0.499999999999998);
#3774=CIRCLE('',#10667,0.500000000000007);
#3775=CIRCLE('',#10669,0.500000000000007);
#3776=CIRCLE('',#10670,0.499999999999998);
#3777=CIRCLE('',#10672,0.500000000000007);
#3778=CIRCLE('',#10673,0.499999999999998);
#3779=CIRCLE('',#10674,0.499999999999998);
#3780=CIRCLE('',#10676,0.500000000000007);
#3781=CIRCLE('',#10677,1.00000000000001);
#3782=CIRCLE('',#10678,0.499999999999998);
#3783=CIRCLE('',#10682,0.500000000000007);
#3784=CIRCLE('',#10683,0.999999999999996);
#3785=CIRCLE('',#10684,0.500000000000007);
#3786=CIRCLE('',#10716,0.3);
#3787=CIRCLE('',#10717,0.299999999999994);
#3788=CIRCLE('',#10719,0.300000000000011);
#3789=CIRCLE('',#10720,4.79999999999999);
#3790=CIRCLE('',#10721,4.49999999999999);
#3791=CIRCLE('',#10723,0.300000000000002);
#3792=CIRCLE('',#10725,4.79999999999998);
#3793=CIRCLE('',#10726,4.49999999999998);
#3794=CIRCLE('',#10728,4.49999999999999);
#3795=CIRCLE('',#10732,0.3);
#3796=CIRCLE('',#10733,0.299999999999994);
#3797=CIRCLE('',#10734,0.300000000000011);
#3798=CIRCLE('',#10735,0.599999999999987);
#3799=CIRCLE('',#10737,0.3);
#3800=CIRCLE('',#10738,0.299999999999994);
#3801=CIRCLE('',#10739,0.300000000000011);
#3802=CIRCLE('',#10741,0.600000000000001);
#3803=CIRCLE('',#10742,0.299999999999976);
#3804=CIRCLE('',#10743,0.3);
#3805=CIRCLE('',#10744,0.300000000000011);
#3806=CIRCLE('',#10748,0.300000000000003);
#3807=CIRCLE('',#10749,0.3);
#3808=CIRCLE('',#10750,0.300000000000011);
#3809=CIRCLE('',#10752,0.3);
#3810=CIRCLE('',#10753,0.299999999999994);
#3811=CIRCLE('',#10754,0.300000000000011);
#3812=CIRCLE('',#10757,0.299999999999994);
#3813=CIRCLE('',#10758,0.3);
#3814=CIRCLE('',#10759,0.300000000000011);
#3815=CIRCLE('',#10761,0.300000000000006);
#3816=CIRCLE('',#10762,0.300000000000011);
#3817=CIRCLE('',#10763,0.3);
#3818=CIRCLE('',#10765,0.3);
#3819=CIRCLE('',#10766,0.300000000000003);
#3820=CIRCLE('',#10767,0.300000000000011);
#3821=CIRCLE('',#10769,0.300000000000011);
#3822=CIRCLE('',#10770,0.299999999999994);
#3823=CIRCLE('',#10771,0.3);
#3824=CIRCLE('',#10774,0.3);
#3825=CIRCLE('',#10775,0.300000000000011);
#3826=CIRCLE('',#10776,0.300000000000001);
#3827=CIRCLE('',#10796,4.79999999999998);
#3828=CIRCLE('',#10797,4.79999999999999);
#3829=CIRCLE('',#10801,0.3);
#3830=CIRCLE('',#10802,0.299999999999994);
#3831=CIRCLE('',#10804,0.300000000000002);
#3832=CIRCLE('',#10805,4.49999999999998);
#3833=CIRCLE('',#10807,0.300000000000002);
#3834=CIRCLE('',#10814,8.);
#3835=CIRCLE('',#10815,7.5);
#3836=CIRCLE('',#10817,8.);
#3837=CIRCLE('',#10818,9.);
#3838=CIRCLE('',#10820,9.);
#3839=CIRCLE('',#10824,7.5);
#3840=CIRCLE('',#10828,0.3);
#3841=CIRCLE('',#10829,0.299999999999994);
#3842=CIRCLE('',#10831,0.300000000000011);
#3843=CIRCLE('',#10832,4.49999999999999);
#3844=CIRCLE('',#10833,4.79999999999999);
#3845=CIRCLE('',#10835,0.300000000000002);
#3846=CIRCLE('',#10837,4.49999999999998);
#3847=CIRCLE('',#10838,4.79999999999998);
#3848=CIRCLE('',#10840,4.49999999999999);
#3849=CIRCLE('',#10844,0.3);
#3850=CIRCLE('',#10845,0.599999999999987);
#3851=CIRCLE('',#10846,0.300000000000011);
#3852=CIRCLE('',#10847,0.299999999999994);
#3853=CIRCLE('',#10849,0.3);
#3854=CIRCLE('',#10850,0.300000000000011);
#3855=CIRCLE('',#10851,0.299999999999994);
#3856=CIRCLE('',#10853,0.600000000000001);
#3857=CIRCLE('',#10854,0.300000000000011);
#3858=CIRCLE('',#10855,0.3);
#3859=CIRCLE('',#10856,0.299999999999976);
#3860=CIRCLE('',#10860,0.300000000000003);
#3861=CIRCLE('',#10861,0.300000000000011);
#3862=CIRCLE('',#10862,0.3);
#3863=CIRCLE('',#10864,0.3);
#3864=CIRCLE('',#10865,0.300000000000011);
#3865=CIRCLE('',#10866,0.299999999999994);
#3866=CIRCLE('',#10869,0.299999999999994);
#3867=CIRCLE('',#10870,0.300000000000011);
#3868=CIRCLE('',#10871,0.3);
#3869=CIRCLE('',#10873,0.300000000000006);
#3870=CIRCLE('',#10874,0.3);
#3871=CIRCLE('',#10875,0.300000000000011);
#3872=CIRCLE('',#10877,0.3);
#3873=CIRCLE('',#10878,0.300000000000011);
#3874=CIRCLE('',#10879,0.300000000000003);
#3875=CIRCLE('',#10881,0.300000000000011);
#3876=CIRCLE('',#10882,0.3);
#3877=CIRCLE('',#10883,0.299999999999994);
#3878=CIRCLE('',#10886,0.3);
#3879=CIRCLE('',#10887,0.300000000000001);
#3880=CIRCLE('',#10888,0.300000000000011);
#3881=CIRCLE('',#10908,4.79999999999999);
#3882=CIRCLE('',#10909,4.79999999999998);
#3883=CIRCLE('',#10913,0.3);
#3884=CIRCLE('',#10914,0.299999999999994);
#3885=CIRCLE('',#10916,0.300000000000002);
#3886=CIRCLE('',#10917,4.49999999999998);
#3887=CIRCLE('',#10919,0.300000000000002);
#3888=CIRCLE('',#10926,0.3);
#3889=CIRCLE('',#10927,0.299999999999994);
#3890=CIRCLE('',#10929,0.300000000000011);
#3891=CIRCLE('',#10930,4.79999999999999);
#3892=CIRCLE('',#10931,4.49999999999999);
#3893=CIRCLE('',#10933,0.300000000000002);
#3894=CIRCLE('',#10935,4.79999999999998);
#3895=CIRCLE('',#10936,4.49999999999998);
#3896=CIRCLE('',#10938,4.49999999999999);
#3897=CIRCLE('',#10942,0.3);
#3898=CIRCLE('',#10943,0.299999999999994);
#3899=CIRCLE('',#10944,0.300000000000011);
#3900=CIRCLE('',#10945,0.599999999999987);
#3901=CIRCLE('',#10947,0.3);
#3902=CIRCLE('',#10948,0.299999999999994);
#3903=CIRCLE('',#10949,0.300000000000011);
#3904=CIRCLE('',#10951,0.600000000000001);
#3905=CIRCLE('',#10952,0.299999999999976);
#3906=CIRCLE('',#10953,0.3);
#3907=CIRCLE('',#10954,0.300000000000011);
#3908=CIRCLE('',#10958,0.300000000000003);
#3909=CIRCLE('',#10959,0.3);
#3910=CIRCLE('',#10960,0.300000000000011);
#3911=CIRCLE('',#10962,0.3);
#3912=CIRCLE('',#10963,0.299999999999994);
#3913=CIRCLE('',#10964,0.300000000000011);
#3914=CIRCLE('',#10967,0.299999999999994);
#3915=CIRCLE('',#10968,0.3);
#3916=CIRCLE('',#10969,0.300000000000011);
#3917=CIRCLE('',#10971,0.300000000000006);
#3918=CIRCLE('',#10972,0.300000000000011);
#3919=CIRCLE('',#10973,0.3);
#3920=CIRCLE('',#10975,0.3);
#3921=CIRCLE('',#10976,0.300000000000003);
#3922=CIRCLE('',#10977,0.300000000000011);
#3923=CIRCLE('',#10979,0.300000000000011);
#3924=CIRCLE('',#10980,0.299999999999994);
#3925=CIRCLE('',#10981,0.3);
#3926=CIRCLE('',#10984,0.3);
#3927=CIRCLE('',#10985,0.300000000000011);
#3928=CIRCLE('',#10986,0.300000000000001);
#3929=CIRCLE('',#11006,4.79999999999998);
#3930=CIRCLE('',#11007,4.79999999999999);
#3931=CIRCLE('',#11011,0.3);
#3932=CIRCLE('',#11012,0.299999999999994);
#3933=CIRCLE('',#11014,0.300000000000002);
#3934=CIRCLE('',#11015,4.49999999999998);
#3935=CIRCLE('',#11017,0.300000000000002);
#3936=VERTEX_POINT('',#14266);
#3937=VERTEX_POINT('',#14268);
#3938=VERTEX_POINT('',#14271);
#3939=VERTEX_POINT('',#14273);
#3940=VERTEX_POINT('',#14277);
#3941=VERTEX_POINT('',#14284);
#3942=VERTEX_POINT('',#14290);
#3943=VERTEX_POINT('',#14291);
#3944=VERTEX_POINT('',#14293);
#3945=VERTEX_POINT('',#14295);
#3946=VERTEX_POINT('',#14297);
#3947=VERTEX_POINT('',#14299);
#3948=VERTEX_POINT('',#14303);
#3949=VERTEX_POINT('',#14304);
#3950=VERTEX_POINT('',#14306);
#3951=VERTEX_POINT('',#14308);
#3952=VERTEX_POINT('',#14310);
#3953=VERTEX_POINT('',#14312);
#3954=VERTEX_POINT('',#14319);
#3955=VERTEX_POINT('',#14321);
#3956=VERTEX_POINT('',#14325);
#3957=VERTEX_POINT('',#14327);
#3958=VERTEX_POINT('',#14331);
#3959=VERTEX_POINT('',#14335);
#3960=VERTEX_POINT('',#14339);
#3961=VERTEX_POINT('',#14343);
#3962=VERTEX_POINT('',#14347);
#3963=VERTEX_POINT('',#14349);
#3964=VERTEX_POINT('',#14351);
#3965=VERTEX_POINT('',#14353);
#3966=VERTEX_POINT('',#14355);
#3967=VERTEX_POINT('',#14357);
#3968=VERTEX_POINT('',#14359);
#3969=VERTEX_POINT('',#14361);
#3970=VERTEX_POINT('',#14363);
#3971=VERTEX_POINT('',#14365);
#3972=VERTEX_POINT('',#14367);
#3973=VERTEX_POINT('',#14369);
#3974=VERTEX_POINT('',#14371);
#3975=VERTEX_POINT('',#14373);
#3976=VERTEX_POINT('',#14375);
#3977=VERTEX_POINT('',#14377);
#3978=VERTEX_POINT('',#14379);
#3979=VERTEX_POINT('',#14381);
#3980=VERTEX_POINT('',#14385);
#3981=VERTEX_POINT('',#14387);
#3982=VERTEX_POINT('',#14389);
#3983=VERTEX_POINT('',#14391);
#3984=VERTEX_POINT('',#14395);
#3985=VERTEX_POINT('',#14397);
#3986=VERTEX_POINT('',#14399);
#3987=VERTEX_POINT('',#14401);
#3988=VERTEX_POINT('',#14407);
#3989=VERTEX_POINT('',#14411);
#3990=VERTEX_POINT('',#14413);
#3991=VERTEX_POINT('',#14415);
#3992=VERTEX_POINT('',#14417);
#3993=VERTEX_POINT('',#14419);
#3994=VERTEX_POINT('',#14421);
#3995=VERTEX_POINT('',#14423);
#3996=VERTEX_POINT('',#14425);
#3997=VERTEX_POINT('',#14427);
#3998=VERTEX_POINT('',#14429);
#3999=VERTEX_POINT('',#14431);
#4000=VERTEX_POINT('',#14433);
#4001=VERTEX_POINT('',#14435);
#4002=VERTEX_POINT('',#14438);
#4003=VERTEX_POINT('',#14442);
#4004=VERTEX_POINT('',#14446);
#4005=VERTEX_POINT('',#14450);
#4006=VERTEX_POINT('',#14452);
#4007=VERTEX_POINT('',#14456);
#4008=VERTEX_POINT('',#14458);
#4009=VERTEX_POINT('',#14462);
#4010=VERTEX_POINT('',#14464);
#4011=VERTEX_POINT('',#14468);
#4012=VERTEX_POINT('',#14470);
#4013=VERTEX_POINT('',#14476);
#4014=VERTEX_POINT('',#14478);
#4015=VERTEX_POINT('',#14487);
#4016=VERTEX_POINT('',#14489);
#4017=VERTEX_POINT('',#14498);
#4018=VERTEX_POINT('',#14500);
#4019=VERTEX_POINT('',#14504);
#4020=VERTEX_POINT('',#14508);
#4021=VERTEX_POINT('',#14510);
#4022=VERTEX_POINT('',#14519);
#4023=VERTEX_POINT('',#14523);
#4024=VERTEX_POINT('',#14525);
#4025=VERTEX_POINT('',#14529);
#4026=VERTEX_POINT('',#14531);
#4027=VERTEX_POINT('',#14540);
#4028=VERTEX_POINT('',#14542);
#4029=VERTEX_POINT('',#14546);
#4030=VERTEX_POINT('',#14548);
#4031=VERTEX_POINT('',#14554);
#4032=VERTEX_POINT('',#14556);
#4033=VERTEX_POINT('',#14565);
#4034=VERTEX_POINT('',#14574);
#4035=VERTEX_POINT('',#14576);
#4036=VERTEX_POINT('',#14580);
#4037=VERTEX_POINT('',#14586);
#4038=VERTEX_POINT('',#14588);
#4039=VERTEX_POINT('',#14592);
#4040=VERTEX_POINT('',#14598);
#4041=VERTEX_POINT('',#14599);
#4042=VERTEX_POINT('',#14608);
#4043=VERTEX_POINT('',#14610);
#4044=VERTEX_POINT('',#14659);
#4045=VERTEX_POINT('',#14661);
#4046=VERTEX_POINT('',#14665);
#4047=VERTEX_POINT('',#14667);
#4048=VERTEX_POINT('',#14672);
#4049=VERTEX_POINT('',#14674);
#4050=VERTEX_POINT('',#14679);
#4051=VERTEX_POINT('',#14681);
#4052=VERTEX_POINT('',#14685);
#4053=VERTEX_POINT('',#14686);
#4054=VERTEX_POINT('',#14688);
#4055=VERTEX_POINT('',#14692);
#4056=VERTEX_POINT('',#14693);
#4057=VERTEX_POINT('',#14695);
#4058=VERTEX_POINT('',#14699);
#4059=VERTEX_POINT('',#14700);
#4060=VERTEX_POINT('',#14702);
#4061=VERTEX_POINT('',#14704);
#4062=VERTEX_POINT('',#14711);
#4063=VERTEX_POINT('',#14712);
#4064=VERTEX_POINT('',#14714);
#4065=VERTEX_POINT('',#14716);
#4066=VERTEX_POINT('',#14720);
#4067=VERTEX_POINT('',#14721);
#4068=VERTEX_POINT('',#14723);
#4069=VERTEX_POINT('',#14725);
#4070=VERTEX_POINT('',#14729);
#4071=VERTEX_POINT('',#14730);
#4072=VERTEX_POINT('',#14732);
#4073=VERTEX_POINT('',#14734);
#4074=VERTEX_POINT('',#14741);
#4075=VERTEX_POINT('',#14742);
#4076=VERTEX_POINT('',#14744);
#4077=VERTEX_POINT('',#14751);
#4078=VERTEX_POINT('',#14752);
#4079=VERTEX_POINT('',#14754);
#4080=VERTEX_POINT('',#14761);
#4081=VERTEX_POINT('',#14762);
#4082=VERTEX_POINT('',#14764);
#4083=VERTEX_POINT('',#14768);
#4084=VERTEX_POINT('',#14769);
#4085=VERTEX_POINT('',#14771);
#4086=VERTEX_POINT('',#14778);
#4087=VERTEX_POINT('',#14779);
#4088=VERTEX_POINT('',#14781);
#4089=VERTEX_POINT('',#14788);
#4090=VERTEX_POINT('',#14789);
#4091=VERTEX_POINT('',#14791);
#4092=VERTEX_POINT('',#14798);
#4093=VERTEX_POINT('',#14799);
#4094=VERTEX_POINT('',#14801);
#4095=VERTEX_POINT('',#14805);
#4096=VERTEX_POINT('',#14806);
#4097=VERTEX_POINT('',#14808);
#4098=VERTEX_POINT('',#14815);
#4099=VERTEX_POINT('',#14816);
#4100=VERTEX_POINT('',#14818);
#4101=VERTEX_POINT('',#14820);
#4102=VERTEX_POINT('',#14827);
#4103=VERTEX_POINT('',#14828);
#4104=VERTEX_POINT('',#14830);
#4105=VERTEX_POINT('',#14834);
#4106=VERTEX_POINT('',#14835);
#4107=VERTEX_POINT('',#14837);
#4108=VERTEX_POINT('',#14839);
#4109=VERTEX_POINT('',#14843);
#4110=VERTEX_POINT('',#14844);
#4111=VERTEX_POINT('',#14846);
#4112=VERTEX_POINT('',#14850);
#4113=VERTEX_POINT('',#14851);
#4114=VERTEX_POINT('',#14853);
#4115=VERTEX_POINT('',#14860);
#4116=VERTEX_POINT('',#14861);
#4117=VERTEX_POINT('',#14863);
#4118=VERTEX_POINT('',#14867);
#4119=VERTEX_POINT('',#14868);
#4120=VERTEX_POINT('',#14870);
#4121=VERTEX_POINT('',#14874);
#4122=VERTEX_POINT('',#14875);
#4123=VERTEX_POINT('',#14877);
#4124=VERTEX_POINT('',#14881);
#4125=VERTEX_POINT('',#14882);
#4126=VERTEX_POINT('',#14884);
#4127=VERTEX_POINT('',#14886);
#4128=VERTEX_POINT('',#14896);
#4129=VERTEX_POINT('',#14897);
#4130=VERTEX_POINT('',#14899);
#4131=VERTEX_POINT('',#14901);
#4132=VERTEX_POINT('',#14992);
#4133=VERTEX_POINT('',#14994);
#4134=VERTEX_POINT('',#14999);
#4135=VERTEX_POINT('',#15001);
#4136=VERTEX_POINT('',#15006);
#4137=VERTEX_POINT('',#15008);
#4138=VERTEX_POINT('',#15013);
#4139=VERTEX_POINT('',#15015);
#4140=VERTEX_POINT('',#15020);
#4141=VERTEX_POINT('',#15022);
#4142=VERTEX_POINT('',#15027);
#4143=VERTEX_POINT('',#15029);
#4144=VERTEX_POINT('',#15034);
#4145=VERTEX_POINT('',#15036);
#4146=VERTEX_POINT('',#15041);
#4147=VERTEX_POINT('',#15043);
#4148=VERTEX_POINT('',#15048);
#4149=VERTEX_POINT('',#15049);
#4150=VERTEX_POINT('',#15051);
#4151=VERTEX_POINT('',#15053);
#4152=VERTEX_POINT('',#15055);
#4153=VERTEX_POINT('',#15057);
#4154=VERTEX_POINT('',#15061);
#4155=VERTEX_POINT('',#15062);
#4156=VERTEX_POINT('',#15064);
#4157=VERTEX_POINT('',#15066);
#4158=VERTEX_POINT('',#15068);
#4159=VERTEX_POINT('',#15070);
#4160=VERTEX_POINT('',#15077);
#4161=VERTEX_POINT('',#15079);
#4162=VERTEX_POINT('',#15083);
#4163=VERTEX_POINT('',#15085);
#4164=VERTEX_POINT('',#15089);
#4165=VERTEX_POINT('',#15093);
#4166=VERTEX_POINT('',#15097);
#4167=VERTEX_POINT('',#15101);
#4168=VERTEX_POINT('',#15105);
#4169=VERTEX_POINT('',#15107);
#4170=VERTEX_POINT('',#15109);
#4171=VERTEX_POINT('',#15111);
#4172=VERTEX_POINT('',#15113);
#4173=VERTEX_POINT('',#15115);
#4174=VERTEX_POINT('',#15117);
#4175=VERTEX_POINT('',#15119);
#4176=VERTEX_POINT('',#15121);
#4177=VERTEX_POINT('',#15123);
#4178=VERTEX_POINT('',#15125);
#4179=VERTEX_POINT('',#15127);
#4180=VERTEX_POINT('',#15129);
#4181=VERTEX_POINT('',#15131);
#4182=VERTEX_POINT('',#15133);
#4183=VERTEX_POINT('',#15135);
#4184=VERTEX_POINT('',#15137);
#4185=VERTEX_POINT('',#15139);
#4186=VERTEX_POINT('',#15143);
#4187=VERTEX_POINT('',#15145);
#4188=VERTEX_POINT('',#15147);
#4189=VERTEX_POINT('',#15149);
#4190=VERTEX_POINT('',#15153);
#4191=VERTEX_POINT('',#15155);
#4192=VERTEX_POINT('',#15157);
#4193=VERTEX_POINT('',#15159);
#4194=VERTEX_POINT('',#15165);
#4195=VERTEX_POINT('',#15169);
#4196=VERTEX_POINT('',#15171);
#4197=VERTEX_POINT('',#15173);
#4198=VERTEX_POINT('',#15175);
#4199=VERTEX_POINT('',#15177);
#4200=VERTEX_POINT('',#15179);
#4201=VERTEX_POINT('',#15181);
#4202=VERTEX_POINT('',#15183);
#4203=VERTEX_POINT('',#15185);
#4204=VERTEX_POINT('',#15187);
#4205=VERTEX_POINT('',#15189);
#4206=VERTEX_POINT('',#15191);
#4207=VERTEX_POINT('',#15193);
#4208=VERTEX_POINT('',#15196);
#4209=VERTEX_POINT('',#15200);
#4210=VERTEX_POINT('',#15204);
#4211=VERTEX_POINT('',#15208);
#4212=VERTEX_POINT('',#15210);
#4213=VERTEX_POINT('',#15214);
#4214=VERTEX_POINT('',#15216);
#4215=VERTEX_POINT('',#15220);
#4216=VERTEX_POINT('',#15222);
#4217=VERTEX_POINT('',#15226);
#4218=VERTEX_POINT('',#15228);
#4219=VERTEX_POINT('',#15234);
#4220=VERTEX_POINT('',#15236);
#4221=VERTEX_POINT('',#15245);
#4222=VERTEX_POINT('',#15247);
#4223=VERTEX_POINT('',#15256);
#4224=VERTEX_POINT('',#15258);
#4225=VERTEX_POINT('',#15262);
#4226=VERTEX_POINT('',#15266);
#4227=VERTEX_POINT('',#15268);
#4228=VERTEX_POINT('',#15277);
#4229=VERTEX_POINT('',#15281);
#4230=VERTEX_POINT('',#15283);
#4231=VERTEX_POINT('',#15287);
#4232=VERTEX_POINT('',#15289);
#4233=VERTEX_POINT('',#15298);
#4234=VERTEX_POINT('',#15300);
#4235=VERTEX_POINT('',#15304);
#4236=VERTEX_POINT('',#15306);
#4237=VERTEX_POINT('',#15312);
#4238=VERTEX_POINT('',#15314);
#4239=VERTEX_POINT('',#15323);
#4240=VERTEX_POINT('',#15332);
#4241=VERTEX_POINT('',#15334);
#4242=VERTEX_POINT('',#15338);
#4243=VERTEX_POINT('',#15344);
#4244=VERTEX_POINT('',#15346);
#4245=VERTEX_POINT('',#15350);
#4246=VERTEX_POINT('',#15356);
#4247=VERTEX_POINT('',#15357);
#4248=VERTEX_POINT('',#15366);
#4249=VERTEX_POINT('',#15368);
#4250=VERTEX_POINT('',#15417);
#4251=VERTEX_POINT('',#15418);
#4252=VERTEX_POINT('',#15420);
#4253=VERTEX_POINT('',#15422);
#4254=VERTEX_POINT('',#15426);
#4255=VERTEX_POINT('',#15427);
#4256=VERTEX_POINT('',#15432);
#4257=VERTEX_POINT('',#15433);
#4258=VERTEX_POINT('',#15441);
#4259=VERTEX_POINT('',#15443);
#4260=VERTEX_POINT('',#15447);
#4261=VERTEX_POINT('',#15451);
#4262=VERTEX_POINT('',#15452);
#4263=VERTEX_POINT('',#15454);
#4264=VERTEX_POINT('',#15456);
#4265=VERTEX_POINT('',#15460);
#4266=VERTEX_POINT('',#15462);
#4267=VERTEX_POINT('',#15464);
#4268=VERTEX_POINT('',#15468);
#4269=VERTEX_POINT('',#15469);
#4270=VERTEX_POINT('',#15471);
#4271=VERTEX_POINT('',#15475);
#4272=VERTEX_POINT('',#15476);
#4273=VERTEX_POINT('',#15479);
#4274=VERTEX_POINT('',#15483);
#4275=VERTEX_POINT('',#15485);
#4276=VERTEX_POINT('',#15489);
#4277=VERTEX_POINT('',#15490);
#4278=VERTEX_POINT('',#15495);
#4279=VERTEX_POINT('',#15496);
#4280=VERTEX_POINT('',#15498);
#4281=VERTEX_POINT('',#15505);
#4282=VERTEX_POINT('',#15506);
#4283=VERTEX_POINT('',#15508);
#4284=VERTEX_POINT('',#15512);
#4285=VERTEX_POINT('',#15514);
#4286=VERTEX_POINT('',#15518);
#4287=VERTEX_POINT('',#15519);
#4288=VERTEX_POINT('',#15521);
#4289=VERTEX_POINT('',#15525);
#4290=VERTEX_POINT('',#15526);
#4291=VERTEX_POINT('',#15528);
#4292=VERTEX_POINT('',#15535);
#4293=VERTEX_POINT('',#15536);
#4294=VERTEX_POINT('',#15538);
#4295=VERTEX_POINT('',#15574);
#4296=VERTEX_POINT('',#15576);
#4297=VERTEX_POINT('',#15587);
#4298=VERTEX_POINT('',#15588);
#4299=VERTEX_POINT('',#15590);
#4300=VERTEX_POINT('',#15592);
#4301=VERTEX_POINT('',#15601);
#4302=VERTEX_POINT('',#15614);
#4303=VERTEX_POINT('',#15616);
#4304=VERTEX_POINT('',#15620);
#4305=VERTEX_POINT('',#15622);
#4306=VERTEX_POINT('',#15624);
#4307=VERTEX_POINT('',#15626);
#4308=VERTEX_POINT('',#15637);
#4309=VERTEX_POINT('',#15639);
#4310=VERTEX_POINT('',#15650);
#4311=VERTEX_POINT('',#15652);
#4312=VERTEX_POINT('',#15663);
#4313=VERTEX_POINT('',#15665);
#4314=VERTEX_POINT('',#15678);
#4315=VERTEX_POINT('',#15680);
#4316=VERTEX_POINT('',#15682);
#4317=VERTEX_POINT('',#15684);
#4318=VERTEX_POINT('',#15686);
#4319=VERTEX_POINT('',#15688);
#4320=VERTEX_POINT('',#15690);
#4321=VERTEX_POINT('',#15692);
#4322=VERTEX_POINT('',#15694);
#4323=VERTEX_POINT('',#15696);
#4324=VERTEX_POINT('',#15698);
#4325=VERTEX_POINT('',#15700);
#4326=VERTEX_POINT('',#15702);
#4327=VERTEX_POINT('',#15704);
#4328=VERTEX_POINT('',#15706);
#4329=VERTEX_POINT('',#15708);
#4330=VERTEX_POINT('',#15710);
#4331=VERTEX_POINT('',#15712);
#4332=VERTEX_POINT('',#15714);
#4333=VERTEX_POINT('',#15716);
#4334=VERTEX_POINT('',#15718);
#4335=VERTEX_POINT('',#15720);
#4336=VERTEX_POINT('',#15722);
#4337=VERTEX_POINT('',#15726);
#4338=VERTEX_POINT('',#15730);
#4339=VERTEX_POINT('',#15734);
#4340=VERTEX_POINT('',#15738);
#4341=VERTEX_POINT('',#15741);
#4342=VERTEX_POINT('',#15752);
#4343=VERTEX_POINT('',#15754);
#4344=VERTEX_POINT('',#15765);
#4345=VERTEX_POINT('',#15767);
#4346=VERTEX_POINT('',#15778);
#4347=VERTEX_POINT('',#15791);
#4348=VERTEX_POINT('',#15793);
#4349=VERTEX_POINT('',#15797);
#4350=VERTEX_POINT('',#15799);
#4351=VERTEX_POINT('',#15803);
#4352=VERTEX_POINT('',#15805);
#4353=VERTEX_POINT('',#15807);
#4354=VERTEX_POINT('',#15809);
#4355=VERTEX_POINT('',#15820);
#4356=VERTEX_POINT('',#15832);
#4357=VERTEX_POINT('',#15843);
#4358=VERTEX_POINT('',#15845);
#4359=VERTEX_POINT('',#15858);
#4360=VERTEX_POINT('',#15860);
#4361=VERTEX_POINT('',#15864);
#4362=VERTEX_POINT('',#15866);
#4363=VERTEX_POINT('',#15868);
#4364=VERTEX_POINT('',#15870);
#4365=VERTEX_POINT('',#15881);
#4366=VERTEX_POINT('',#15893);
#4367=VERTEX_POINT('',#15904);
#4368=VERTEX_POINT('',#15906);
#4369=VERTEX_POINT('',#15919);
#4370=VERTEX_POINT('',#15921);
#4371=VERTEX_POINT('',#15925);
#4372=VERTEX_POINT('',#15927);
#4373=VERTEX_POINT('',#15929);
#4374=VERTEX_POINT('',#15931);
#4375=VERTEX_POINT('',#15942);
#4376=VERTEX_POINT('',#15954);
#4377=VERTEX_POINT('',#15965);
#4378=VERTEX_POINT('',#15967);
#4379=VERTEX_POINT('',#15980);
#4380=VERTEX_POINT('',#15982);
#4381=VERTEX_POINT('',#15986);
#4382=VERTEX_POINT('',#15989);
#4383=VERTEX_POINT('',#16000);
#4384=VERTEX_POINT('',#16002);
#4385=VERTEX_POINT('',#16013);
#4386=VERTEX_POINT('',#16015);
#4387=VERTEX_POINT('',#16026);
#4388=VERTEX_POINT('',#16039);
#4389=VERTEX_POINT('',#16041);
#4390=VERTEX_POINT('',#16045);
#4391=VERTEX_POINT('',#16047);
#4392=VERTEX_POINT('',#16049);
#4393=VERTEX_POINT('',#16051);
#4394=VERTEX_POINT('',#16062);
#4395=VERTEX_POINT('',#16074);
#4396=VERTEX_POINT('',#16085);
#4397=VERTEX_POINT('',#16087);
#4398=VERTEX_POINT('',#16100);
#4399=VERTEX_POINT('',#16102);
#4400=VERTEX_POINT('',#16104);
#4401=VERTEX_POINT('',#16106);
#4402=VERTEX_POINT('',#16117);
#4403=VERTEX_POINT('',#16119);
#4404=VERTEX_POINT('',#16130);
#4405=VERTEX_POINT('',#16132);
#4406=VERTEX_POINT('',#16143);
#4407=VERTEX_POINT('',#16145);
#4408=VERTEX_POINT('',#16156);
#4409=VERTEX_POINT('',#16158);
#4410=VERTEX_POINT('',#16180);
#4411=VERTEX_POINT('',#16182);
#4412=VERTEX_POINT('',#16199);
#4413=VERTEX_POINT('',#16201);
#4414=VERTEX_POINT('',#16218);
#4415=VERTEX_POINT('',#16220);
#4416=VERTEX_POINT('',#16244);
#4417=VERTEX_POINT('',#16246);
#4418=VERTEX_POINT('',#16248);
#4419=VERTEX_POINT('',#16250);
#4420=VERTEX_POINT('',#16261);
#4421=VERTEX_POINT('',#16273);
#4422=VERTEX_POINT('',#16284);
#4423=VERTEX_POINT('',#16286);
#4424=VERTEX_POINT('',#16299);
#4425=VERTEX_POINT('',#16301);
#4426=VERTEX_POINT('',#16303);
#4427=VERTEX_POINT('',#16305);
#4428=VERTEX_POINT('',#16316);
#4429=VERTEX_POINT('',#16318);
#4430=VERTEX_POINT('',#16329);
#4431=VERTEX_POINT('',#16331);
#4432=VERTEX_POINT('',#16342);
#4433=VERTEX_POINT('',#16344);
#4434=VERTEX_POINT('',#16355);
#4435=VERTEX_POINT('',#16357);
#4436=VERTEX_POINT('',#16379);
#4437=VERTEX_POINT('',#16381);
#4438=VERTEX_POINT('',#16398);
#4439=VERTEX_POINT('',#16400);
#4440=VERTEX_POINT('',#16417);
#4441=VERTEX_POINT('',#16419);
#4442=VERTEX_POINT('',#16443);
#4443=VERTEX_POINT('',#16445);
#4444=VERTEX_POINT('',#16447);
#4445=VERTEX_POINT('',#16449);
#4446=VERTEX_POINT('',#16460);
#4447=VERTEX_POINT('',#16462);
#4448=VERTEX_POINT('',#16473);
#4449=VERTEX_POINT('',#16475);
#4450=VERTEX_POINT('',#16486);
#4451=VERTEX_POINT('',#16488);
#4452=VERTEX_POINT('',#16499);
#4453=VERTEX_POINT('',#16501);
#4454=VERTEX_POINT('',#16523);
#4455=VERTEX_POINT('',#16525);
#4456=VERTEX_POINT('',#16542);
#4457=VERTEX_POINT('',#16544);
#4458=VERTEX_POINT('',#16561);
#4459=VERTEX_POINT('',#16563);
#4460=VERTEX_POINT('',#16587);
#4461=VERTEX_POINT('',#16589);
#4462=VERTEX_POINT('',#16591);
#4463=VERTEX_POINT('',#16593);
#4464=VERTEX_POINT('',#16604);
#4465=VERTEX_POINT('',#16606);
#4466=VERTEX_POINT('',#16617);
#4467=VERTEX_POINT('',#16619);
#4468=VERTEX_POINT('',#16630);
#4469=VERTEX_POINT('',#16632);
#4470=VERTEX_POINT('',#16643);
#4471=VERTEX_POINT('',#16645);
#4472=VERTEX_POINT('',#16667);
#4473=VERTEX_POINT('',#16669);
#4474=VERTEX_POINT('',#16686);
#4475=VERTEX_POINT('',#16688);
#4476=VERTEX_POINT('',#16705);
#4477=VERTEX_POINT('',#16707);
#4478=VERTEX_POINT('',#16731);
#4479=VERTEX_POINT('',#16733);
#4480=VERTEX_POINT('',#16737);
#4481=VERTEX_POINT('',#16740);
#4482=VERTEX_POINT('',#16751);
#4483=VERTEX_POINT('',#16753);
#4484=VERTEX_POINT('',#16764);
#4485=VERTEX_POINT('',#16766);
#4486=VERTEX_POINT('',#16777);
#4487=VERTEX_POINT('',#16792);
#4488=VERTEX_POINT('',#16798);
#4489=VERTEX_POINT('',#16804);
#4490=VERTEX_POINT('',#16810);
#4491=VERTEX_POINT('',#16818);
#4492=VERTEX_POINT('',#16824);
#4493=VERTEX_POINT('',#16828);
#4494=VERTEX_POINT('',#16830);
#4495=VERTEX_POINT('',#16837);
#4496=VERTEX_POINT('',#16839);
#4497=VERTEX_POINT('',#16849);
#4498=VERTEX_POINT('',#16855);
#4499=VERTEX_POINT('',#16863);
#4500=VERTEX_POINT('',#16865);
#4501=VERTEX_POINT('',#16872);
#4502=VERTEX_POINT('',#16874);
#4503=VERTEX_POINT('',#16881);
#4504=VERTEX_POINT('',#16887);
#4505=VERTEX_POINT('',#16895);
#4506=VERTEX_POINT('',#16901);
#4507=VERTEX_POINT('',#16907);
#4508=VERTEX_POINT('',#16911);
#4509=VERTEX_POINT('',#16929);
#4510=VERTEX_POINT('',#16931);
#4511=VERTEX_POINT('',#16933);
#4512=VERTEX_POINT('',#16939);
#4513=VERTEX_POINT('',#16949);
#4514=VERTEX_POINT('',#16969);
#4515=VERTEX_POINT('',#16971);
#4516=VERTEX_POINT('',#16975);
#4517=VERTEX_POINT('',#16979);
#4518=VERTEX_POINT('',#16983);
#4519=VERTEX_POINT('',#16985);
#4520=VERTEX_POINT('',#16991);
#4521=VERTEX_POINT('',#16992);
#4522=VERTEX_POINT('',#16997);
#4523=VERTEX_POINT('',#16999);
#4524=VERTEX_POINT('',#17003);
#4525=VERTEX_POINT('',#17004);
#4526=VERTEX_POINT('',#17011);
#4527=VERTEX_POINT('',#17017);
#4528=VERTEX_POINT('',#17018);
#4529=VERTEX_POINT('',#17025);
#4530=VERTEX_POINT('',#17029);
#4531=VERTEX_POINT('',#17031);
#4532=VERTEX_POINT('',#17037);
#4533=VERTEX_POINT('',#17043);
#4534=VERTEX_POINT('',#17044);
#4535=VERTEX_POINT('',#17046);
#4536=VERTEX_POINT('',#17053);
#4537=VERTEX_POINT('',#17057);
#4538=VERTEX_POINT('',#17058);
#4539=VERTEX_POINT('',#17060);
#4540=VERTEX_POINT('',#17067);
#4541=VERTEX_POINT('',#17069);
#4542=VERTEX_POINT('',#17075);
#4543=VERTEX_POINT('',#17076);
#4544=VERTEX_POINT('',#17078);
#4545=VERTEX_POINT('',#17082);
#4546=VERTEX_POINT('',#17084);
#4547=VERTEX_POINT('',#17088);
#4548=VERTEX_POINT('',#17089);
#4549=VERTEX_POINT('',#17091);
#4550=VERTEX_POINT('',#17095);
#4551=VERTEX_POINT('',#17101);
#4552=VERTEX_POINT('',#17102);
#4553=VERTEX_POINT('',#17107);
#4554=VERTEX_POINT('',#17111);
#4555=VERTEX_POINT('',#17112);
#4556=VERTEX_POINT('',#17117);
#4557=VERTEX_POINT('',#17119);
#4558=VERTEX_POINT('',#17127);
#4559=VERTEX_POINT('',#17129);
#4560=VERTEX_POINT('',#17190);
#4561=VERTEX_POINT('',#17191);
#4562=VERTEX_POINT('',#17193);
#4563=VERTEX_POINT('',#17195);
#4564=VERTEX_POINT('',#17199);
#4565=VERTEX_POINT('',#17200);
#4566=VERTEX_POINT('',#17205);
#4567=VERTEX_POINT('',#17206);
#4568=VERTEX_POINT('',#17214);
#4569=VERTEX_POINT('',#17216);
#4570=VERTEX_POINT('',#17220);
#4571=VERTEX_POINT('',#17224);
#4572=VERTEX_POINT('',#17225);
#4573=VERTEX_POINT('',#17227);
#4574=VERTEX_POINT('',#17229);
#4575=VERTEX_POINT('',#17233);
#4576=VERTEX_POINT('',#17235);
#4577=VERTEX_POINT('',#17237);
#4578=VERTEX_POINT('',#17241);
#4579=VERTEX_POINT('',#17242);
#4580=VERTEX_POINT('',#17244);
#4581=VERTEX_POINT('',#17248);
#4582=VERTEX_POINT('',#17249);
#4583=VERTEX_POINT('',#17251);
#4584=VERTEX_POINT('',#17256);
#4585=VERTEX_POINT('',#17258);
#4586=VERTEX_POINT('',#17262);
#4587=VERTEX_POINT('',#17263);
#4588=VERTEX_POINT('',#17268);
#4589=VERTEX_POINT('',#17269);
#4590=VERTEX_POINT('',#17271);
#4591=VERTEX_POINT('',#17278);
#4592=VERTEX_POINT('',#17279);
#4593=VERTEX_POINT('',#17281);
#4594=VERTEX_POINT('',#17285);
#4595=VERTEX_POINT('',#17287);
#4596=VERTEX_POINT('',#17291);
#4597=VERTEX_POINT('',#17292);
#4598=VERTEX_POINT('',#17294);
#4599=VERTEX_POINT('',#17298);
#4600=VERTEX_POINT('',#17299);
#4601=VERTEX_POINT('',#17301);
#4602=VERTEX_POINT('',#17308);
#4603=VERTEX_POINT('',#17309);
#4604=VERTEX_POINT('',#17311);
#4605=VERTEX_POINT('',#17347);
#4606=VERTEX_POINT('',#17349);
#4607=VERTEX_POINT('',#17360);
#4608=VERTEX_POINT('',#17361);
#4609=VERTEX_POINT('',#17363);
#4610=VERTEX_POINT('',#17365);
#4611=VERTEX_POINT('',#17374);
#4612=VERTEX_POINT('',#17387);
#4613=VERTEX_POINT('',#17389);
#4614=VERTEX_POINT('',#17392);
#4615=VERTEX_POINT('',#17394);
#4616=VERTEX_POINT('',#17398);
#4617=VERTEX_POINT('',#17405);
#4618=VERTEX_POINT('',#17411);
#4619=VERTEX_POINT('',#17412);
#4620=VERTEX_POINT('',#17414);
#4621=VERTEX_POINT('',#17416);
#4622=VERTEX_POINT('',#17420);
#4623=VERTEX_POINT('',#17421);
#4624=VERTEX_POINT('',#17426);
#4625=VERTEX_POINT('',#17427);
#4626=VERTEX_POINT('',#17435);
#4627=VERTEX_POINT('',#17437);
#4628=VERTEX_POINT('',#17441);
#4629=VERTEX_POINT('',#17445);
#4630=VERTEX_POINT('',#17446);
#4631=VERTEX_POINT('',#17448);
#4632=VERTEX_POINT('',#17450);
#4633=VERTEX_POINT('',#17454);
#4634=VERTEX_POINT('',#17456);
#4635=VERTEX_POINT('',#17458);
#4636=VERTEX_POINT('',#17462);
#4637=VERTEX_POINT('',#17463);
#4638=VERTEX_POINT('',#17465);
#4639=VERTEX_POINT('',#17469);
#4640=VERTEX_POINT('',#17470);
#4641=VERTEX_POINT('',#17473);
#4642=VERTEX_POINT('',#17477);
#4643=VERTEX_POINT('',#17479);
#4644=VERTEX_POINT('',#17483);
#4645=VERTEX_POINT('',#17484);
#4646=VERTEX_POINT('',#17489);
#4647=VERTEX_POINT('',#17490);
#4648=VERTEX_POINT('',#17492);
#4649=VERTEX_POINT('',#17499);
#4650=VERTEX_POINT('',#17500);
#4651=VERTEX_POINT('',#17502);
#4652=VERTEX_POINT('',#17506);
#4653=VERTEX_POINT('',#17508);
#4654=VERTEX_POINT('',#17512);
#4655=VERTEX_POINT('',#17513);
#4656=VERTEX_POINT('',#17515);
#4657=VERTEX_POINT('',#17519);
#4658=VERTEX_POINT('',#17520);
#4659=VERTEX_POINT('',#17522);
#4660=VERTEX_POINT('',#17529);
#4661=VERTEX_POINT('',#17530);
#4662=VERTEX_POINT('',#17532);
#4663=VERTEX_POINT('',#17568);
#4664=VERTEX_POINT('',#17570);
#4665=VERTEX_POINT('',#17581);
#4666=VERTEX_POINT('',#17582);
#4667=VERTEX_POINT('',#17584);
#4668=VERTEX_POINT('',#17586);
#4669=VERTEX_POINT('',#17595);
#4670=VERTEX_POINT('',#17608);
#4671=VERTEX_POINT('',#17609);
#4672=VERTEX_POINT('',#17611);
#4673=VERTEX_POINT('',#17613);
#4674=VERTEX_POINT('',#17617);
#4675=VERTEX_POINT('',#17618);
#4676=VERTEX_POINT('',#17623);
#4677=VERTEX_POINT('',#17624);
#4678=VERTEX_POINT('',#17632);
#4679=VERTEX_POINT('',#17634);
#4680=VERTEX_POINT('',#17638);
#4681=VERTEX_POINT('',#17642);
#4682=VERTEX_POINT('',#17643);
#4683=VERTEX_POINT('',#17645);
#4684=VERTEX_POINT('',#17647);
#4685=VERTEX_POINT('',#17651);
#4686=VERTEX_POINT('',#17653);
#4687=VERTEX_POINT('',#17655);
#4688=VERTEX_POINT('',#17659);
#4689=VERTEX_POINT('',#17660);
#4690=VERTEX_POINT('',#17662);
#4691=VERTEX_POINT('',#17666);
#4692=VERTEX_POINT('',#17667);
#4693=VERTEX_POINT('',#17669);
#4694=VERTEX_POINT('',#17674);
#4695=VERTEX_POINT('',#17676);
#4696=VERTEX_POINT('',#17680);
#4697=VERTEX_POINT('',#17681);
#4698=VERTEX_POINT('',#17686);
#4699=VERTEX_POINT('',#17687);
#4700=VERTEX_POINT('',#17689);
#4701=VERTEX_POINT('',#17696);
#4702=VERTEX_POINT('',#17697);
#4703=VERTEX_POINT('',#17699);
#4704=VERTEX_POINT('',#17703);
#4705=VERTEX_POINT('',#17705);
#4706=VERTEX_POINT('',#17709);
#4707=VERTEX_POINT('',#17710);
#4708=VERTEX_POINT('',#17712);
#4709=VERTEX_POINT('',#17716);
#4710=VERTEX_POINT('',#17717);
#4711=VERTEX_POINT('',#17719);
#4712=VERTEX_POINT('',#17726);
#4713=VERTEX_POINT('',#17727);
#4714=VERTEX_POINT('',#17729);
#4715=VERTEX_POINT('',#17765);
#4716=VERTEX_POINT('',#17767);
#4717=VERTEX_POINT('',#17778);
#4718=VERTEX_POINT('',#17779);
#4719=VERTEX_POINT('',#17781);
#4720=VERTEX_POINT('',#17783);
#4721=VERTEX_POINT('',#17792);
#4722=EDGE_CURVE('',#3936,#3936,#3308,.T.);
#4723=EDGE_CURVE('',#3937,#3937,#3309,.T.);
#4724=EDGE_CURVE('',#3938,#3938,#3310,.T.);
#4725=EDGE_CURVE('',#3938,#3939,#640,.T.);
#4726=EDGE_CURVE('',#3939,#3939,#3311,.T.);
#4727=EDGE_CURVE('',#3939,#3940,#641,.T.);
#4728=EDGE_CURVE('',#3940,#3940,#3312,.T.);
#4729=EDGE_CURVE('',#3940,#3936,#642,.T.);
#4730=EDGE_CURVE('',#3937,#3941,#643,.T.);
#4731=EDGE_CURVE('',#3941,#3941,#3313,.T.);
#4732=EDGE_CURVE('',#3942,#3943,#3314,.T.);
#4733=EDGE_CURVE('',#3944,#3942,#644,.T.);
#4734=EDGE_CURVE('',#3944,#3945,#645,.T.);
#4735=EDGE_CURVE('',#3946,#3945,#646,.T.);
#4736=EDGE_CURVE('',#3947,#3946,#3315,.T.);
#4737=EDGE_CURVE('',#3943,#3947,#647,.T.);
#4738=EDGE_CURVE('',#3948,#3949,#3316,.T.);
#4739=EDGE_CURVE('',#3950,#3948,#648,.T.);
#4740=EDGE_CURVE('',#3951,#3950,#3317,.T.);
#4741=EDGE_CURVE('',#3952,#3951,#649,.T.);
#4742=EDGE_CURVE('',#3953,#3952,#650,.T.);
#4743=EDGE_CURVE('',#3949,#3953,#651,.T.);
#4744=EDGE_CURVE('',#3945,#3952,#652,.T.);
#4745=EDGE_CURVE('',#3953,#3944,#653,.T.);
#4746=EDGE_CURVE('',#3949,#3954,#654,.T.);
#4747=EDGE_CURVE('',#3954,#3955,#267,.T.);
#4748=EDGE_CURVE('',#3955,#3948,#655,.T.);
#4749=EDGE_CURVE('',#3943,#3956,#656,.T.);
#4750=EDGE_CURVE('',#3956,#3957,#3318,.F.);
#4751=EDGE_CURVE('',#3957,#3942,#657,.T.);
#4752=EDGE_CURVE('',#3955,#3958,#658,.T.);
#4753=EDGE_CURVE('',#3950,#3958,#659,.T.);
#4754=EDGE_CURVE('',#3959,#3947,#660,.T.);
#4755=EDGE_CURVE('',#3956,#3959,#661,.T.);
#4756=EDGE_CURVE('',#3960,#3958,#268,.T.);
#4757=EDGE_CURVE('',#3960,#3951,#662,.T.);
#4758=EDGE_CURVE('',#3946,#3961,#663,.T.);
#4759=EDGE_CURVE('',#3961,#3959,#3319,.F.);
#4760=EDGE_CURVE('',#3962,#3960,#664,.T.);
#4761=EDGE_CURVE('',#3963,#3962,#665,.T.);
#4762=EDGE_CURVE('',#3963,#3964,#666,.T.);
#4763=EDGE_CURVE('',#3964,#3965,#667,.T.);
#4764=EDGE_CURVE('',#3965,#3966,#668,.T.);
#4765=EDGE_CURVE('',#3967,#3966,#669,.T.);
#4766=EDGE_CURVE('',#3968,#3967,#670,.T.);
#4767=EDGE_CURVE('',#3969,#3968,#671,.T.);
#4768=EDGE_CURVE('',#3970,#3969,#3320,.T.);
#4769=EDGE_CURVE('',#3971,#3970,#672,.T.);
#4770=EDGE_CURVE('',#3972,#3971,#673,.T.);
#4771=EDGE_CURVE('',#3973,#3972,#3321,.T.);
#4772=EDGE_CURVE('',#3974,#3973,#674,.T.);
#4773=EDGE_CURVE('',#3975,#3974,#3322,.T.);
#4774=EDGE_CURVE('',#3976,#3975,#675,.T.);
#4775=EDGE_CURVE('',#3977,#3976,#676,.T.);
#4776=EDGE_CURVE('',#3978,#3977,#3323,.T.);
#4777=EDGE_CURVE('',#3979,#3978,#677,.T.);
#4778=EDGE_CURVE('',#3961,#3979,#678,.T.);
#4779=EDGE_CURVE('',#3966,#3980,#3324,.T.);
#4780=EDGE_CURVE('',#3981,#3965,#679,.T.);
#4781=EDGE_CURVE('',#3982,#3981,#680,.T.);
#4782=EDGE_CURVE('',#3983,#3982,#3325,.T.);
#4783=EDGE_CURVE('',#3980,#3983,#681,.T.);
#4784=EDGE_CURVE('',#3984,#3963,#3326,.T.);
#4785=EDGE_CURVE('',#3985,#3984,#682,.T.);
#4786=EDGE_CURVE('',#3986,#3985,#3327,.T.);
#4787=EDGE_CURVE('',#3987,#3986,#683,.T.);
#4788=EDGE_CURVE('',#3987,#3964,#684,.T.);
#4789=EDGE_CURVE('',#3981,#3987,#685,.T.);
#4790=EDGE_CURVE('',#3980,#3988,#686,.T.);
#4791=EDGE_CURVE('',#3988,#3967,#3328,.F.);
#4792=EDGE_CURVE('',#3989,#3957,#687,.T.);
#4793=EDGE_CURVE('',#3990,#3989,#688,.T.);
#4794=EDGE_CURVE('',#3991,#3990,#3329,.T.);
#4795=EDGE_CURVE('',#3992,#3991,#689,.T.);
#4796=EDGE_CURVE('',#3993,#3992,#690,.T.);
#4797=EDGE_CURVE('',#3994,#3993,#3330,.T.);
#4798=EDGE_CURVE('',#3995,#3994,#691,.T.);
#4799=EDGE_CURVE('',#3996,#3995,#3331,.T.);
#4800=EDGE_CURVE('',#3997,#3996,#692,.T.);
#4801=EDGE_CURVE('',#3998,#3997,#693,.T.);
#4802=EDGE_CURVE('',#3999,#3998,#3332,.T.);
#4803=EDGE_CURVE('',#4000,#3999,#694,.T.);
#4804=EDGE_CURVE('',#4001,#4000,#695,.T.);
#4805=EDGE_CURVE('',#3982,#4001,#696,.T.);
#4806=EDGE_CURVE('',#4002,#3986,#697,.T.);
#4807=EDGE_CURVE('',#3954,#4002,#698,.T.);
#4808=EDGE_CURVE('',#4003,#3983,#699,.T.);
#4809=EDGE_CURVE('',#3988,#4003,#700,.T.);
#4810=EDGE_CURVE('',#3985,#4004,#701,.T.);
#4811=EDGE_CURVE('',#4004,#4002,#3333,.F.);
#4812=EDGE_CURVE('',#4005,#3977,#3334,.T.);
#4813=EDGE_CURVE('',#4006,#4005,#3335,.F.);
#4814=EDGE_CURVE('',#3978,#4006,#3336,.T.);
#4815=EDGE_CURVE('',#4007,#3990,#3337,.T.);
#4816=EDGE_CURVE('',#4008,#4007,#3338,.F.);
#4817=EDGE_CURVE('',#3991,#4008,#3339,.T.);
#4818=EDGE_CURVE('',#3976,#4009,#3340,.F.);
#4819=EDGE_CURVE('',#4010,#3976,#3341,.F.);
#4820=EDGE_CURVE('',#4009,#4010,#3342,.F.);
#4821=EDGE_CURVE('',#3979,#4011,#3343,.F.);
#4822=EDGE_CURVE('',#4012,#3979,#3344,.F.);
#4823=EDGE_CURVE('',#4011,#4012,#3345,.F.);
#4824=EDGE_CURVE('',#4006,#4012,#702,.T.);
#4825=EDGE_CURVE('',#3992,#4013,#3346,.F.);
#4826=EDGE_CURVE('',#4014,#3992,#3347,.F.);
#4827=EDGE_CURVE('',#4013,#4014,#3348,.F.);
#4828=EDGE_CURVE('',#4008,#4014,#703,.T.);
#4829=EDGE_CURVE('',#4014,#4009,#704,.T.);
#4830=EDGE_CURVE('',#4010,#4013,#705,.T.);
#4831=EDGE_CURVE('',#4015,#3989,#3349,.F.);
#4832=EDGE_CURVE('',#4016,#4015,#3350,.F.);
#4833=EDGE_CURVE('',#3989,#4016,#3351,.F.);
#4834=EDGE_CURVE('',#4015,#4011,#706,.T.);
#4835=EDGE_CURVE('',#4012,#4016,#707,.T.);
#4836=EDGE_CURVE('',#4016,#4007,#708,.T.);
#4837=EDGE_CURVE('',#4017,#3974,#3352,.T.);
#4838=EDGE_CURVE('',#4018,#4017,#3353,.F.);
#4839=EDGE_CURVE('',#3975,#4018,#3354,.T.);
#4840=EDGE_CURVE('',#3959,#4019,#3355,.F.);
#4841=EDGE_CURVE('',#4019,#3961,#3356,.F.);
#4842=EDGE_CURVE('',#4020,#3993,#3357,.T.);
#4843=EDGE_CURVE('',#4021,#4020,#3358,.F.);
#4844=EDGE_CURVE('',#3994,#4021,#3359,.T.);
#4845=EDGE_CURVE('',#4013,#4020,#709,.T.);
#4846=EDGE_CURVE('',#4020,#4018,#710,.T.);
#4847=EDGE_CURVE('',#4017,#4021,#711,.T.);
#4848=EDGE_CURVE('',#3957,#4022,#3360,.F.);
#4849=EDGE_CURVE('',#4022,#3956,#3361,.F.);
#4850=EDGE_CURVE('',#4023,#3972,#3362,.T.);
#4851=EDGE_CURVE('',#4024,#4023,#3363,.F.);
#4852=EDGE_CURVE('',#3973,#4024,#3364,.T.);
#4853=EDGE_CURVE('',#4025,#3995,#3365,.T.);
#4854=EDGE_CURVE('',#4026,#4025,#3366,.F.);
#4855=EDGE_CURVE('',#3996,#4026,#3367,.T.);
#4856=EDGE_CURVE('',#4021,#4025,#712,.T.);
#4857=EDGE_CURVE('',#4025,#4024,#713,.T.);
#4858=EDGE_CURVE('',#4023,#4026,#714,.T.);
#4859=EDGE_CURVE('',#3971,#4027,#3368,.F.);
#4860=EDGE_CURVE('',#4028,#3971,#3369,.F.);
#4861=EDGE_CURVE('',#4027,#4028,#3370,.F.);
#4862=EDGE_CURVE('',#3962,#4029,#3371,.F.);
#4863=EDGE_CURVE('',#4030,#3962,#3372,.F.);
#4864=EDGE_CURVE('',#4029,#4030,#3373,.F.);
#4865=EDGE_CURVE('',#3958,#4030,#715,.T.);
#4866=EDGE_CURVE('',#3997,#4031,#3374,.F.);
#4867=EDGE_CURVE('',#4032,#3997,#3375,.F.);
#4868=EDGE_CURVE('',#4031,#4032,#3376,.F.);
#4869=EDGE_CURVE('',#4026,#4032,#716,.T.);
#4870=EDGE_CURVE('',#4032,#4027,#717,.T.);
#4871=EDGE_CURVE('',#4028,#4031,#718,.T.);
#4872=EDGE_CURVE('',#4033,#4004,#3377,.F.);
#4873=EDGE_CURVE('',#4002,#4033,#3378,.F.);
#4874=EDGE_CURVE('',#4004,#4029,#719,.T.);
#4875=EDGE_CURVE('',#4030,#4033,#720,.T.);
#4876=EDGE_CURVE('',#4033,#3955,#721,.T.);
#4877=EDGE_CURVE('',#4034,#3969,#3379,.T.);
#4878=EDGE_CURVE('',#4035,#4034,#3380,.F.);
#4879=EDGE_CURVE('',#3970,#4035,#3381,.T.);
#4880=EDGE_CURVE('',#3967,#4036,#3382,.F.);
#4881=EDGE_CURVE('',#4036,#3988,#3383,.F.);
#4882=EDGE_CURVE('',#4029,#3984,#722,.T.);
#4883=EDGE_CURVE('',#4037,#3998,#3384,.T.);
#4884=EDGE_CURVE('',#4038,#4037,#3385,.F.);
#4885=EDGE_CURVE('',#3999,#4038,#3386,.T.);
#4886=EDGE_CURVE('',#4003,#4039,#3387,.F.);
#4887=EDGE_CURVE('',#4001,#4003,#3388,.F.);
#4888=EDGE_CURVE('',#4039,#4001,#3389,.F.);
#4889=EDGE_CURVE('',#4040,#4041,#3390,.F.);
#4890=EDGE_CURVE('',#3968,#4040,#3391,.F.);
#4891=EDGE_CURVE('',#4041,#3968,#3392,.F.);
#4892=EDGE_CURVE('',#4040,#4034,#723,.T.);
#4893=EDGE_CURVE('',#4036,#4041,#724,.T.);
#4894=EDGE_CURVE('',#4042,#4000,#3393,.F.);
#4895=EDGE_CURVE('',#4043,#4042,#3394,.F.);
#4896=EDGE_CURVE('',#4000,#4043,#3395,.F.);
#4897=EDGE_CURVE('',#4041,#4043,#725,.T.);
#4898=EDGE_CURVE('',#4042,#4040,#726,.T.);
#4899=EDGE_CURVE('',#4043,#4039,#727,.T.);
#4900=EDGE_CURVE('',#4038,#4042,#728,.T.);
#4901=EDGE_CURVE('',#4039,#4036,#729,.T.);
#4902=EDGE_CURVE('',#4031,#4037,#730,.T.);
#4903=EDGE_CURVE('',#4037,#4035,#731,.T.);
#4904=EDGE_CURVE('',#4034,#4038,#732,.T.);
#4905=EDGE_CURVE('',#4035,#4028,#733,.T.);
#4906=EDGE_CURVE('',#4027,#4023,#734,.T.);
#4907=EDGE_CURVE('',#4024,#4017,#735,.T.);
#4908=EDGE_CURVE('',#4019,#4022,#736,.T.);
#4909=EDGE_CURVE('',#4022,#4015,#737,.T.);
#4910=EDGE_CURVE('',#4011,#4019,#738,.T.);
#4911=EDGE_CURVE('',#4018,#4010,#739,.T.);
#4912=EDGE_CURVE('',#4009,#4005,#740,.T.);
#4913=EDGE_CURVE('',#4007,#4006,#741,.T.);
#4914=EDGE_CURVE('',#4005,#4008,#742,.T.);
#4915=EDGE_CURVE('',#4044,#4044,#3396,.T.);
#4916=EDGE_CURVE('',#4044,#4045,#743,.T.);
#4917=EDGE_CURVE('',#4045,#4045,#3397,.T.);
#4918=EDGE_CURVE('',#4046,#4046,#3398,.T.);
#4919=EDGE_CURVE('',#4046,#4047,#744,.T.);
#4920=EDGE_CURVE('',#4047,#4047,#3399,.T.);
#4921=EDGE_CURVE('',#4048,#4048,#3400,.T.);
#4922=EDGE_CURVE('',#4048,#4049,#745,.T.);
#4923=EDGE_CURVE('',#4049,#4049,#3401,.T.);
#4924=EDGE_CURVE('',#4050,#4050,#3402,.T.);
#4925=EDGE_CURVE('',#4050,#4051,#746,.T.);
#4926=EDGE_CURVE('',#4051,#4051,#3403,.T.);
#4927=EDGE_CURVE('',#4052,#4053,#3404,.F.);
#4928=EDGE_CURVE('',#4054,#4052,#3405,.F.);
#4929=EDGE_CURVE('',#4053,#4054,#3406,.F.);
#4930=EDGE_CURVE('',#4055,#4056,#3407,.F.);
#4931=EDGE_CURVE('',#4057,#4055,#3408,.F.);
#4932=EDGE_CURVE('',#4056,#4057,#3409,.F.);
#4933=EDGE_CURVE('',#4058,#4059,#3410,.F.);
#4934=EDGE_CURVE('',#4060,#4058,#3411,.T.);
#4935=EDGE_CURVE('',#4060,#4061,#3412,.T.);
#4936=EDGE_CURVE('',#4059,#4061,#3413,.T.);
#4937=EDGE_CURVE('',#4058,#4053,#747,.T.);
#4938=EDGE_CURVE('',#4054,#4060,#748,.T.);
#4939=EDGE_CURVE('',#4062,#4063,#3414,.T.);
#4940=EDGE_CURVE('',#4064,#4063,#3415,.T.);
#4941=EDGE_CURVE('',#4065,#4064,#3416,.F.);
#4942=EDGE_CURVE('',#4062,#4065,#3417,.T.);
#4943=EDGE_CURVE('',#4066,#4067,#3418,.F.);
#4944=EDGE_CURVE('',#4068,#4066,#3419,.T.);
#4945=EDGE_CURVE('',#4068,#4069,#3420,.T.);
#4946=EDGE_CURVE('',#4067,#4069,#3421,.T.);
#4947=EDGE_CURVE('',#4070,#4071,#3422,.T.);
#4948=EDGE_CURVE('',#4072,#4071,#3423,.T.);
#4949=EDGE_CURVE('',#4073,#4072,#3424,.F.);
#4950=EDGE_CURVE('',#4070,#4073,#3425,.T.);
#4951=EDGE_CURVE('',#4073,#4057,#749,.T.);
#4952=EDGE_CURVE('',#4055,#4070,#750,.T.);
#4953=EDGE_CURVE('',#4074,#4075,#3426,.F.);
#4954=EDGE_CURVE('',#4076,#4074,#3427,.F.);
#4955=EDGE_CURVE('',#4075,#4076,#3428,.F.);
#4956=EDGE_CURVE('',#4074,#4059,#751,.T.);
#4957=EDGE_CURVE('',#4061,#4076,#752,.T.);
#4958=EDGE_CURVE('',#4077,#4078,#3429,.F.);
#4959=EDGE_CURVE('',#4079,#4077,#3430,.F.);
#4960=EDGE_CURVE('',#4078,#4079,#3431,.F.);
#4961=EDGE_CURVE('',#4077,#4062,#753,.T.);
#4962=EDGE_CURVE('',#4065,#4079,#754,.T.);
#4963=EDGE_CURVE('',#4080,#4081,#3432,.F.);
#4964=EDGE_CURVE('',#4082,#4080,#3433,.F.);
#4965=EDGE_CURVE('',#4081,#4082,#3434,.F.);
#4966=EDGE_CURVE('',#4083,#4084,#3435,.F.);
#4967=EDGE_CURVE('',#4085,#4083,#3436,.F.);
#4968=EDGE_CURVE('',#4084,#4085,#3437,.F.);
#4969=EDGE_CURVE('',#4071,#4085,#755,.T.);
#4970=EDGE_CURVE('',#4083,#4072,#756,.T.);
#4971=EDGE_CURVE('',#4086,#4087,#3438,.F.);
#4972=EDGE_CURVE('',#4088,#4086,#3439,.F.);
#4973=EDGE_CURVE('',#4087,#4088,#3440,.F.);
#4974=EDGE_CURVE('',#4086,#4075,#757,.T.);
#4975=EDGE_CURVE('',#4076,#4088,#758,.T.);
#4976=EDGE_CURVE('',#4089,#4090,#3441,.F.);
#4977=EDGE_CURVE('',#4091,#4089,#3442,.F.);
#4978=EDGE_CURVE('',#4090,#4091,#3443,.F.);
#4979=EDGE_CURVE('',#4089,#4077,#759,.T.);
#4980=EDGE_CURVE('',#4078,#4091,#760,.T.);
#4981=EDGE_CURVE('',#4092,#4093,#3444,.F.);
#4982=EDGE_CURVE('',#4094,#4092,#3445,.F.);
#4983=EDGE_CURVE('',#4093,#4094,#3446,.F.);
#4984=EDGE_CURVE('',#4095,#4096,#3447,.F.);
#4985=EDGE_CURVE('',#4097,#4095,#3448,.F.);
#4986=EDGE_CURVE('',#4096,#4097,#3449,.F.);
#4987=EDGE_CURVE('',#4095,#4084,#761,.T.);
#4988=EDGE_CURVE('',#4085,#4097,#762,.T.);
#4989=EDGE_CURVE('',#4098,#4099,#3450,.F.);
#4990=EDGE_CURVE('',#4100,#4098,#3451,.T.);
#4991=EDGE_CURVE('',#4100,#4101,#3452,.T.);
#4992=EDGE_CURVE('',#4099,#4101,#3453,.T.);
#4993=EDGE_CURVE('',#4098,#4087,#763,.T.);
#4994=EDGE_CURVE('',#4088,#4100,#764,.T.);
#4995=EDGE_CURVE('',#4102,#4103,#3454,.F.);
#4996=EDGE_CURVE('',#4104,#4102,#3455,.F.);
#4997=EDGE_CURVE('',#4103,#4104,#3456,.F.);
#4998=EDGE_CURVE('',#4105,#4106,#3457,.F.);
#4999=EDGE_CURVE('',#4107,#4105,#3458,.T.);
#5000=EDGE_CURVE('',#4107,#4108,#3459,.T.);
#5001=EDGE_CURVE('',#4106,#4108,#3460,.T.);
#5002=EDGE_CURVE('',#4109,#4110,#3461,.F.);
#5003=EDGE_CURVE('',#4111,#4109,#3462,.F.);
#5004=EDGE_CURVE('',#4110,#4111,#3463,.F.);
#5005=EDGE_CURVE('',#4112,#4113,#3464,.F.);
#5006=EDGE_CURVE('',#4114,#4112,#3465,.F.);
#5007=EDGE_CURVE('',#4113,#4114,#3466,.F.);
#5008=EDGE_CURVE('',#4112,#4099,#765,.T.);
#5009=EDGE_CURVE('',#4101,#4114,#766,.T.);
#5010=EDGE_CURVE('',#4115,#4116,#3467,.F.);
#5011=EDGE_CURVE('',#4117,#4115,#3468,.F.);
#5012=EDGE_CURVE('',#4116,#4117,#3469,.F.);
#5013=EDGE_CURVE('',#4118,#4119,#3470,.F.);
#5014=EDGE_CURVE('',#4120,#4118,#3471,.F.);
#5015=EDGE_CURVE('',#4119,#4120,#3472,.F.);
#5016=EDGE_CURVE('',#4121,#4122,#3473,.F.);
#5017=EDGE_CURVE('',#4123,#4121,#3474,.F.);
#5018=EDGE_CURVE('',#4122,#4123,#3475,.F.);
#5019=EDGE_CURVE('',#4124,#4125,#3476,.F.);
#5020=EDGE_CURVE('',#4126,#4124,#3477,.T.);
#5021=EDGE_CURVE('',#4126,#4127,#3478,.T.);
#5022=EDGE_CURVE('',#4125,#4127,#3479,.T.);
#5023=EDGE_CURVE('',#4124,#4113,#767,.T.);
#5024=EDGE_CURVE('',#4114,#4126,#768,.T.);
#5025=EDGE_CURVE('',#4127,#4116,#769,.T.);
#5026=EDGE_CURVE('',#4117,#4125,#770,.T.);
#5027=EDGE_CURVE('',#4128,#4129,#3480,.F.);
#5028=EDGE_CURVE('',#4130,#4128,#3481,.T.);
#5029=EDGE_CURVE('',#4130,#4131,#3482,.T.);
#5030=EDGE_CURVE('',#4129,#4131,#3483,.T.);
#5031=EDGE_CURVE('',#4121,#4130,#771,.T.);
#5032=EDGE_CURVE('',#4128,#4123,#772,.T.);
#5033=EDGE_CURVE('',#4118,#4129,#773,.T.);
#5034=EDGE_CURVE('',#4131,#4120,#774,.T.);
#5035=EDGE_CURVE('',#4125,#4128,#775,.T.);
#5036=EDGE_CURVE('',#4129,#4124,#776,.T.);
#5037=EDGE_CURVE('',#4115,#4122,#777,.T.);
#5038=EDGE_CURVE('',#4123,#4117,#778,.T.);
#5039=EDGE_CURVE('',#4109,#4121,#779,.T.);
#5040=EDGE_CURVE('',#4122,#4111,#780,.T.);
#5041=EDGE_CURVE('',#4105,#4119,#781,.T.);
#5042=EDGE_CURVE('',#4120,#4107,#782,.T.);
#5043=EDGE_CURVE('',#4119,#4112,#783,.T.);
#5044=EDGE_CURVE('',#4113,#4118,#784,.T.);
#5045=EDGE_CURVE('',#4102,#4115,#785,.T.);
#5046=EDGE_CURVE('',#4116,#4104,#786,.T.);
#5047=EDGE_CURVE('',#4103,#4110,#787,.T.);
#5048=EDGE_CURVE('',#4111,#4102,#788,.T.);
#5049=EDGE_CURVE('',#4110,#4096,#789,.T.);
#5050=EDGE_CURVE('',#4097,#4109,#790,.T.);
#5051=EDGE_CURVE('',#4092,#4106,#791,.T.);
#5052=EDGE_CURVE('',#4108,#4094,#792,.T.);
#5053=EDGE_CURVE('',#4106,#4098,#793,.T.);
#5054=EDGE_CURVE('',#4099,#4105,#794,.T.);
#5055=EDGE_CURVE('',#4090,#4103,#795,.T.);
#5056=EDGE_CURVE('',#4104,#4089,#796,.T.);
#5057=EDGE_CURVE('',#4096,#4090,#797,.T.);
#5058=EDGE_CURVE('',#4091,#4095,#798,.T.);
#5059=EDGE_CURVE('',#4080,#4093,#799,.T.);
#5060=EDGE_CURVE('',#4094,#4082,#800,.T.);
#5061=EDGE_CURVE('',#4093,#4086,#801,.T.);
#5062=EDGE_CURVE('',#4087,#4092,#802,.T.);
#5063=EDGE_CURVE('',#4084,#4078,#803,.T.);
#5064=EDGE_CURVE('',#4079,#4083,#804,.T.);
#5065=EDGE_CURVE('',#4066,#4081,#805,.T.);
#5066=EDGE_CURVE('',#4082,#4068,#806,.T.);
#5067=EDGE_CURVE('',#4081,#4074,#807,.T.);
#5068=EDGE_CURVE('',#4075,#4080,#808,.T.);
#5069=EDGE_CURVE('',#4072,#4065,#809,.T.);
#5070=EDGE_CURVE('',#4064,#4073,#810,.T.);
#5071=EDGE_CURVE('',#4056,#4067,#811,.T.);
#5072=EDGE_CURVE('',#4069,#4055,#812,.T.);
#5073=EDGE_CURVE('',#4067,#4058,#813,.T.);
#5074=EDGE_CURVE('',#4059,#4066,#814,.T.);
#5075=EDGE_CURVE('',#4052,#4064,#815,.T.);
#5076=EDGE_CURVE('',#4063,#4054,#816,.T.);
#5077=EDGE_CURVE('',#4057,#4052,#817,.T.);
#5078=EDGE_CURVE('',#4053,#4056,#818,.T.);
#5079=EDGE_CURVE('',#4132,#4132,#3484,.T.);
#5080=EDGE_CURVE('',#4132,#4133,#819,.T.);
#5081=EDGE_CURVE('',#4133,#4133,#3485,.T.);
#5082=EDGE_CURVE('',#4134,#4134,#3486,.T.);
#5083=EDGE_CURVE('',#4134,#4135,#820,.T.);
#5084=EDGE_CURVE('',#4135,#4135,#3487,.T.);
#5085=EDGE_CURVE('',#4136,#4136,#3488,.T.);
#5086=EDGE_CURVE('',#4136,#4137,#821,.T.);
#5087=EDGE_CURVE('',#4137,#4137,#3489,.T.);
#5088=EDGE_CURVE('',#4138,#4138,#3490,.T.);
#5089=EDGE_CURVE('',#4138,#4139,#822,.T.);
#5090=EDGE_CURVE('',#4139,#4139,#3491,.T.);
#5091=EDGE_CURVE('',#4140,#4140,#3492,.T.);
#5092=EDGE_CURVE('',#4140,#4141,#823,.T.);
#5093=EDGE_CURVE('',#4141,#4141,#3493,.T.);
#5094=EDGE_CURVE('',#4142,#4142,#3494,.T.);
#5095=EDGE_CURVE('',#4142,#4143,#824,.T.);
#5096=EDGE_CURVE('',#4143,#4143,#3495,.T.);
#5097=EDGE_CURVE('',#4144,#4144,#3496,.T.);
#5098=EDGE_CURVE('',#4144,#4145,#825,.T.);
#5099=EDGE_CURVE('',#4145,#4145,#3497,.T.);
#5100=EDGE_CURVE('',#4146,#4146,#3498,.T.);
#5101=EDGE_CURVE('',#4146,#4147,#826,.T.);
#5102=EDGE_CURVE('',#4147,#4147,#3499,.T.);
#5103=EDGE_CURVE('',#4148,#4149,#3500,.T.);
#5104=EDGE_CURVE('',#4150,#4148,#827,.T.);
#5105=EDGE_CURVE('',#4150,#4151,#828,.T.);
#5106=EDGE_CURVE('',#4152,#4151,#829,.T.);
#5107=EDGE_CURVE('',#4153,#4152,#3501,.T.);
#5108=EDGE_CURVE('',#4149,#4153,#830,.T.);
#5109=EDGE_CURVE('',#4154,#4155,#3502,.T.);
#5110=EDGE_CURVE('',#4156,#4154,#831,.T.);
#5111=EDGE_CURVE('',#4157,#4156,#3503,.T.);
#5112=EDGE_CURVE('',#4158,#4157,#832,.T.);
#5113=EDGE_CURVE('',#4159,#4158,#833,.T.);
#5114=EDGE_CURVE('',#4155,#4159,#834,.T.);
#5115=EDGE_CURVE('',#4151,#4158,#835,.T.);
#5116=EDGE_CURVE('',#4159,#4150,#836,.T.);
#5117=EDGE_CURVE('',#4155,#4160,#837,.T.);
#5118=EDGE_CURVE('',#4160,#4161,#269,.T.);
#5119=EDGE_CURVE('',#4161,#4154,#838,.T.);
#5120=EDGE_CURVE('',#4149,#4162,#839,.T.);
#5121=EDGE_CURVE('',#4162,#4163,#3504,.F.);
#5122=EDGE_CURVE('',#4163,#4148,#840,.T.);
#5123=EDGE_CURVE('',#4161,#4164,#841,.T.);
#5124=EDGE_CURVE('',#4156,#4164,#842,.T.);
#5125=EDGE_CURVE('',#4165,#4153,#843,.T.);
#5126=EDGE_CURVE('',#4162,#4165,#844,.T.);
#5127=EDGE_CURVE('',#4166,#4164,#270,.T.);
#5128=EDGE_CURVE('',#4166,#4157,#845,.T.);
#5129=EDGE_CURVE('',#4152,#4167,#846,.T.);
#5130=EDGE_CURVE('',#4167,#4165,#3505,.F.);
#5131=EDGE_CURVE('',#4168,#4166,#847,.T.);
#5132=EDGE_CURVE('',#4169,#4168,#848,.T.);
#5133=EDGE_CURVE('',#4169,#4170,#849,.T.);
#5134=EDGE_CURVE('',#4170,#4171,#850,.T.);
#5135=EDGE_CURVE('',#4171,#4172,#851,.T.);
#5136=EDGE_CURVE('',#4173,#4172,#852,.T.);
#5137=EDGE_CURVE('',#4174,#4173,#853,.T.);
#5138=EDGE_CURVE('',#4175,#4174,#854,.T.);
#5139=EDGE_CURVE('',#4176,#4175,#3506,.T.);
#5140=EDGE_CURVE('',#4177,#4176,#855,.T.);
#5141=EDGE_CURVE('',#4178,#4177,#856,.T.);
#5142=EDGE_CURVE('',#4179,#4178,#3507,.T.);
#5143=EDGE_CURVE('',#4180,#4179,#857,.T.);
#5144=EDGE_CURVE('',#4181,#4180,#3508,.T.);
#5145=EDGE_CURVE('',#4182,#4181,#858,.T.);
#5146=EDGE_CURVE('',#4183,#4182,#859,.T.);
#5147=EDGE_CURVE('',#4184,#4183,#3509,.T.);
#5148=EDGE_CURVE('',#4185,#4184,#860,.T.);
#5149=EDGE_CURVE('',#4167,#4185,#861,.T.);
#5150=EDGE_CURVE('',#4172,#4186,#3510,.T.);
#5151=EDGE_CURVE('',#4187,#4171,#862,.T.);
#5152=EDGE_CURVE('',#4188,#4187,#863,.T.);
#5153=EDGE_CURVE('',#4189,#4188,#3511,.T.);
#5154=EDGE_CURVE('',#4186,#4189,#864,.T.);
#5155=EDGE_CURVE('',#4190,#4169,#3512,.T.);
#5156=EDGE_CURVE('',#4191,#4190,#865,.T.);
#5157=EDGE_CURVE('',#4192,#4191,#3513,.T.);
#5158=EDGE_CURVE('',#4193,#4192,#866,.T.);
#5159=EDGE_CURVE('',#4193,#4170,#867,.T.);
#5160=EDGE_CURVE('',#4187,#4193,#868,.T.);
#5161=EDGE_CURVE('',#4186,#4194,#869,.T.);
#5162=EDGE_CURVE('',#4194,#4173,#3514,.F.);
#5163=EDGE_CURVE('',#4195,#4163,#870,.T.);
#5164=EDGE_CURVE('',#4196,#4195,#871,.T.);
#5165=EDGE_CURVE('',#4197,#4196,#3515,.T.);
#5166=EDGE_CURVE('',#4198,#4197,#872,.T.);
#5167=EDGE_CURVE('',#4199,#4198,#873,.T.);
#5168=EDGE_CURVE('',#4200,#4199,#3516,.T.);
#5169=EDGE_CURVE('',#4201,#4200,#874,.T.);
#5170=EDGE_CURVE('',#4202,#4201,#3517,.T.);
#5171=EDGE_CURVE('',#4203,#4202,#875,.T.);
#5172=EDGE_CURVE('',#4204,#4203,#876,.T.);
#5173=EDGE_CURVE('',#4205,#4204,#3518,.T.);
#5174=EDGE_CURVE('',#4206,#4205,#877,.T.);
#5175=EDGE_CURVE('',#4207,#4206,#878,.T.);
#5176=EDGE_CURVE('',#4188,#4207,#879,.T.);
#5177=EDGE_CURVE('',#4208,#4192,#880,.T.);
#5178=EDGE_CURVE('',#4160,#4208,#881,.T.);
#5179=EDGE_CURVE('',#4209,#4189,#882,.T.);
#5180=EDGE_CURVE('',#4194,#4209,#883,.T.);
#5181=EDGE_CURVE('',#4191,#4210,#884,.T.);
#5182=EDGE_CURVE('',#4210,#4208,#3519,.F.);
#5183=EDGE_CURVE('',#4211,#4183,#3520,.T.);
#5184=EDGE_CURVE('',#4212,#4211,#3521,.F.);
#5185=EDGE_CURVE('',#4184,#4212,#3522,.T.);
#5186=EDGE_CURVE('',#4213,#4196,#3523,.T.);
#5187=EDGE_CURVE('',#4214,#4213,#3524,.F.);
#5188=EDGE_CURVE('',#4197,#4214,#3525,.T.);
#5189=EDGE_CURVE('',#4182,#4215,#3526,.F.);
#5190=EDGE_CURVE('',#4216,#4182,#3527,.F.);
#5191=EDGE_CURVE('',#4215,#4216,#3528,.F.);
#5192=EDGE_CURVE('',#4185,#4217,#3529,.F.);
#5193=EDGE_CURVE('',#4218,#4185,#3530,.F.);
#5194=EDGE_CURVE('',#4217,#4218,#3531,.F.);
#5195=EDGE_CURVE('',#4212,#4218,#885,.T.);
#5196=EDGE_CURVE('',#4198,#4219,#3532,.F.);
#5197=EDGE_CURVE('',#4220,#4198,#3533,.F.);
#5198=EDGE_CURVE('',#4219,#4220,#3534,.F.);
#5199=EDGE_CURVE('',#4214,#4220,#886,.T.);
#5200=EDGE_CURVE('',#4220,#4215,#887,.T.);
#5201=EDGE_CURVE('',#4216,#4219,#888,.T.);
#5202=EDGE_CURVE('',#4221,#4195,#3535,.F.);
#5203=EDGE_CURVE('',#4222,#4221,#3536,.F.);
#5204=EDGE_CURVE('',#4195,#4222,#3537,.F.);
#5205=EDGE_CURVE('',#4221,#4217,#889,.T.);
#5206=EDGE_CURVE('',#4218,#4222,#890,.T.);
#5207=EDGE_CURVE('',#4222,#4213,#891,.T.);
#5208=EDGE_CURVE('',#4223,#4180,#3538,.T.);
#5209=EDGE_CURVE('',#4224,#4223,#3539,.F.);
#5210=EDGE_CURVE('',#4181,#4224,#3540,.T.);
#5211=EDGE_CURVE('',#4165,#4225,#3541,.F.);
#5212=EDGE_CURVE('',#4225,#4167,#3542,.F.);
#5213=EDGE_CURVE('',#4226,#4199,#3543,.T.);
#5214=EDGE_CURVE('',#4227,#4226,#3544,.F.);
#5215=EDGE_CURVE('',#4200,#4227,#3545,.T.);
#5216=EDGE_CURVE('',#4219,#4226,#892,.T.);
#5217=EDGE_CURVE('',#4226,#4224,#893,.T.);
#5218=EDGE_CURVE('',#4223,#4227,#894,.T.);
#5219=EDGE_CURVE('',#4163,#4228,#3546,.F.);
#5220=EDGE_CURVE('',#4228,#4162,#3547,.F.);
#5221=EDGE_CURVE('',#4229,#4178,#3548,.T.);
#5222=EDGE_CURVE('',#4230,#4229,#3549,.F.);
#5223=EDGE_CURVE('',#4179,#4230,#3550,.T.);
#5224=EDGE_CURVE('',#4231,#4201,#3551,.T.);
#5225=EDGE_CURVE('',#4232,#4231,#3552,.F.);
#5226=EDGE_CURVE('',#4202,#4232,#3553,.T.);
#5227=EDGE_CURVE('',#4227,#4231,#895,.T.);
#5228=EDGE_CURVE('',#4231,#4230,#896,.T.);
#5229=EDGE_CURVE('',#4229,#4232,#897,.T.);
#5230=EDGE_CURVE('',#4177,#4233,#3554,.F.);
#5231=EDGE_CURVE('',#4234,#4177,#3555,.F.);
#5232=EDGE_CURVE('',#4233,#4234,#3556,.F.);
#5233=EDGE_CURVE('',#4168,#4235,#3557,.F.);
#5234=EDGE_CURVE('',#4236,#4168,#3558,.F.);
#5235=EDGE_CURVE('',#4235,#4236,#3559,.F.);
#5236=EDGE_CURVE('',#4164,#4236,#898,.T.);
#5237=EDGE_CURVE('',#4203,#4237,#3560,.F.);
#5238=EDGE_CURVE('',#4238,#4203,#3561,.F.);
#5239=EDGE_CURVE('',#4237,#4238,#3562,.F.);
#5240=EDGE_CURVE('',#4232,#4238,#899,.T.);
#5241=EDGE_CURVE('',#4238,#4233,#900,.T.);
#5242=EDGE_CURVE('',#4234,#4237,#901,.T.);
#5243=EDGE_CURVE('',#4239,#4210,#3563,.F.);
#5244=EDGE_CURVE('',#4208,#4239,#3564,.F.);
#5245=EDGE_CURVE('',#4210,#4235,#902,.T.);
#5246=EDGE_CURVE('',#4236,#4239,#903,.T.);
#5247=EDGE_CURVE('',#4239,#4161,#904,.T.);
#5248=EDGE_CURVE('',#4240,#4175,#3565,.T.);
#5249=EDGE_CURVE('',#4241,#4240,#3566,.F.);
#5250=EDGE_CURVE('',#4176,#4241,#3567,.T.);
#5251=EDGE_CURVE('',#4173,#4242,#3568,.F.);
#5252=EDGE_CURVE('',#4242,#4194,#3569,.F.);
#5253=EDGE_CURVE('',#4235,#4190,#905,.T.);
#5254=EDGE_CURVE('',#4243,#4204,#3570,.T.);
#5255=EDGE_CURVE('',#4244,#4243,#3571,.F.);
#5256=EDGE_CURVE('',#4205,#4244,#3572,.T.);
#5257=EDGE_CURVE('',#4209,#4245,#3573,.F.);
#5258=EDGE_CURVE('',#4207,#4209,#3574,.F.);
#5259=EDGE_CURVE('',#4245,#4207,#3575,.F.);
#5260=EDGE_CURVE('',#4246,#4247,#3576,.F.);
#5261=EDGE_CURVE('',#4174,#4246,#3577,.F.);
#5262=EDGE_CURVE('',#4247,#4174,#3578,.F.);
#5263=EDGE_CURVE('',#4246,#4240,#906,.T.);
#5264=EDGE_CURVE('',#4242,#4247,#907,.T.);
#5265=EDGE_CURVE('',#4248,#4206,#3579,.F.);
#5266=EDGE_CURVE('',#4249,#4248,#3580,.F.);
#5267=EDGE_CURVE('',#4206,#4249,#3581,.F.);
#5268=EDGE_CURVE('',#4247,#4249,#908,.T.);
#5269=EDGE_CURVE('',#4248,#4246,#909,.T.);
#5270=EDGE_CURVE('',#4249,#4245,#910,.T.);
#5271=EDGE_CURVE('',#4244,#4248,#911,.T.);
#5272=EDGE_CURVE('',#4245,#4242,#912,.T.);
#5273=EDGE_CURVE('',#4237,#4243,#913,.T.);
#5274=EDGE_CURVE('',#4243,#4241,#914,.T.);
#5275=EDGE_CURVE('',#4240,#4244,#915,.T.);
#5276=EDGE_CURVE('',#4241,#4234,#916,.T.);
#5277=EDGE_CURVE('',#4233,#4229,#917,.T.);
#5278=EDGE_CURVE('',#4230,#4223,#918,.T.);
#5279=EDGE_CURVE('',#4225,#4228,#919,.T.);
#5280=EDGE_CURVE('',#4228,#4221,#920,.T.);
#5281=EDGE_CURVE('',#4217,#4225,#921,.T.);
#5282=EDGE_CURVE('',#4224,#4216,#922,.T.);
#5283=EDGE_CURVE('',#4215,#4211,#923,.T.);
#5284=EDGE_CURVE('',#4213,#4212,#924,.T.);
#5285=EDGE_CURVE('',#4211,#4214,#925,.T.);
#5286=EDGE_CURVE('',#4250,#4251,#3582,.T.);
#5287=EDGE_CURVE('',#4252,#4250,#926,.T.);
#5288=EDGE_CURVE('',#4253,#4252,#3583,.T.);
#5289=EDGE_CURVE('',#4251,#4253,#927,.T.);
#5290=EDGE_CURVE('',#4254,#4255,#3584,.T.);
#5291=EDGE_CURVE('',#4253,#4254,#3585,.T.);
#5292=EDGE_CURVE('',#4255,#4252,#3586,.T.);
#5293=EDGE_CURVE('',#4256,#4257,#3587,.T.);
#5294=EDGE_CURVE('',#4254,#4256,#928,.T.);
#5295=EDGE_CURVE('',#4257,#4255,#929,.T.);
#5296=EDGE_CURVE('',#4256,#4251,#3588,.T.);
#5297=EDGE_CURVE('',#4250,#4257,#3589,.T.);
#5298=EDGE_CURVE('',#4258,#4254,#930,.T.);
#5299=EDGE_CURVE('',#4258,#4259,#3590,.T.);
#5300=EDGE_CURVE('',#4259,#4253,#931,.T.);
#5301=EDGE_CURVE('',#4259,#4260,#932,.T.);
#5302=EDGE_CURVE('',#4260,#4251,#933,.T.);
#5303=EDGE_CURVE('',#4261,#4262,#934,.T.);
#5304=EDGE_CURVE('',#4262,#4263,#935,.T.);
#5305=EDGE_CURVE('',#4263,#4264,#936,.T.);
#5306=EDGE_CURVE('',#4264,#4261,#937,.T.);
#5307=EDGE_CURVE('',#4264,#4265,#3591,.T.);
#5308=EDGE_CURVE('',#4266,#4265,#3592,.T.);
#5309=EDGE_CURVE('',#4266,#4267,#3593,.T.);
#5310=EDGE_CURVE('',#4267,#4264,#3594,.F.);
#5311=EDGE_CURVE('',#4268,#4269,#3595,.F.);
#5312=EDGE_CURVE('',#4269,#4270,#3596,.F.);
#5313=EDGE_CURVE('',#4270,#4268,#3597,.F.);
#5314=EDGE_CURVE('',#4271,#4272,#3598,.T.);
#5315=EDGE_CURVE('',#4271,#4261,#3599,.T.);
#5316=EDGE_CURVE('',#4261,#4273,#3600,.F.);
#5317=EDGE_CURVE('',#4273,#4272,#3601,.T.);
#5318=EDGE_CURVE('',#4274,#4273,#938,.T.);
#5319=EDGE_CURVE('',#4275,#4274,#271,.T.);
#5320=EDGE_CURVE('',#4272,#4275,#939,.T.);
#5321=EDGE_CURVE('',#4276,#4277,#3602,.F.);
#5322=EDGE_CURVE('',#4277,#4263,#3603,.F.);
#5323=EDGE_CURVE('',#4263,#4276,#3604,.F.);
#5324=EDGE_CURVE('',#4278,#4279,#3605,.F.);
#5325=EDGE_CURVE('',#4279,#4280,#3606,.F.);
#5326=EDGE_CURVE('',#4280,#4278,#3607,.F.);
#5327=EDGE_CURVE('',#4275,#4280,#940,.T.);
#5328=EDGE_CURVE('',#4278,#4274,#941,.T.);
#5329=EDGE_CURVE('',#4281,#4282,#3608,.F.);
#5330=EDGE_CURVE('',#4282,#4283,#3609,.F.);
#5331=EDGE_CURVE('',#4283,#4281,#3610,.F.);
#5332=EDGE_CURVE('',#4284,#4262,#3611,.F.);
#5333=EDGE_CURVE('',#4262,#4285,#3612,.F.);
#5334=EDGE_CURVE('',#4285,#4284,#3613,.F.);
#5335=EDGE_CURVE('',#4286,#4287,#3614,.F.);
#5336=EDGE_CURVE('',#4287,#4288,#3615,.F.);
#5337=EDGE_CURVE('',#4288,#4286,#3616,.F.);
#5338=EDGE_CURVE('',#4289,#4290,#3617,.F.);
#5339=EDGE_CURVE('',#4290,#4291,#3618,.F.);
#5340=EDGE_CURVE('',#4291,#4289,#3619,.F.);
#5341=EDGE_CURVE('',#4280,#4291,#942,.T.);
#5342=EDGE_CURVE('',#4289,#4279,#943,.T.);
#5343=EDGE_CURVE('',#4292,#4293,#3620,.F.);
#5344=EDGE_CURVE('',#4293,#4294,#3621,.F.);
#5345=EDGE_CURVE('',#4294,#4292,#3622,.F.);
#5346=EDGE_CURVE('',#4292,#4290,#944,.T.);
#5347=EDGE_CURVE('',#4291,#4294,#945,.T.);
#5348=EDGE_CURVE('',#4284,#4293,#946,.T.);
#5349=EDGE_CURVE('',#4294,#4285,#947,.T.);
#5350=EDGE_CURVE('',#4293,#4288,#948,.T.);
#5351=EDGE_CURVE('',#4286,#4292,#949,.T.);
#5352=EDGE_CURVE('',#4290,#4283,#950,.T.);
#5353=EDGE_CURVE('',#4281,#4289,#951,.T.);
#5354=EDGE_CURVE('',#4288,#4276,#952,.T.);
#5355=EDGE_CURVE('',#4277,#4287,#953,.T.);
#5356=EDGE_CURVE('',#4283,#4286,#954,.T.);
#5357=EDGE_CURVE('',#4287,#4282,#955,.T.);
#5358=EDGE_CURVE('',#4285,#4271,#956,.T.);
#5359=EDGE_CURVE('',#4276,#4284,#957,.T.);
#5360=EDGE_CURVE('',#4270,#4281,#958,.T.);
#5361=EDGE_CURVE('',#4282,#4269,#959,.T.);
#5362=EDGE_CURVE('',#4279,#4270,#960,.T.);
#5363=EDGE_CURVE('',#4268,#4278,#961,.T.);
#5364=EDGE_CURVE('',#4265,#4277,#962,.T.);
#5365=EDGE_CURVE('',#4273,#4267,#963,.T.);
#5366=EDGE_CURVE('',#4295,#4268,#964,.T.);
#5367=EDGE_CURVE('',#4296,#4295,#272,.T.);
#5368=EDGE_CURVE('',#4269,#4296,#965,.T.);
#5369=EDGE_CURVE('',#4296,#4266,#966,.T.);
#5370=EDGE_CURVE('',#4267,#4295,#967,.T.);
#5371=EDGE_CURVE('',#4274,#4295,#968,.T.);
#5372=EDGE_CURVE('',#4297,#4298,#969,.T.);
#5373=EDGE_CURVE('',#4298,#4299,#3623,.T.);
#5374=EDGE_CURVE('',#4299,#4300,#970,.T.);
#5375=EDGE_CURVE('',#4300,#4297,#3624,.T.);
#5376=EDGE_CURVE('',#4298,#4259,#3625,.T.);
#5377=EDGE_CURVE('',#4260,#4297,#3626,.T.);
#5378=EDGE_CURVE('',#4301,#4300,#3627,.T.);
#5379=EDGE_CURVE('',#4260,#4301,#3628,.T.);
#5380=EDGE_CURVE('',#4258,#4299,#3629,.T.);
#5381=EDGE_CURVE('',#4301,#4258,#971,.T.);
#5382=EDGE_CURVE('',#4301,#4256,#972,.T.);
#5383=EDGE_CURVE('',#4302,#4302,#3630,.T.);
#5384=EDGE_CURVE('',#4302,#4303,#973,.T.);
#5385=EDGE_CURVE('',#4303,#4303,#3631,.T.);
#5386=EDGE_CURVE('',#4304,#4304,#3632,.T.);
#5387=EDGE_CURVE('',#4304,#4305,#974,.T.);
#5388=EDGE_CURVE('',#4306,#4305,#3633,.T.);
#5389=EDGE_CURVE('',#4307,#4306,#51,.T.);
#5390=EDGE_CURVE('',#4308,#4307,#975,.T.);
#5391=EDGE_CURVE('',#4309,#4308,#52,.T.);
#5392=EDGE_CURVE('',#4310,#4309,#3634,.T.);
#5393=EDGE_CURVE('',#4311,#4310,#53,.T.);
#5394=EDGE_CURVE('',#4312,#4311,#976,.T.);
#5395=EDGE_CURVE('',#4313,#4312,#54,.T.);
#5396=EDGE_CURVE('',#4305,#4313,#3635,.T.);
#5397=EDGE_CURVE('',#4314,#4309,#977,.T.);
#5398=EDGE_CURVE('',#4315,#4314,#978,.T.);
#5399=EDGE_CURVE('',#4316,#4315,#979,.T.);
#5400=EDGE_CURVE('',#4316,#4317,#3636,.T.);
#5401=EDGE_CURVE('',#4318,#4317,#980,.T.);
#5402=EDGE_CURVE('',#4318,#4319,#3637,.T.);
#5403=EDGE_CURVE('',#4320,#4319,#981,.T.);
#5404=EDGE_CURVE('',#4320,#4321,#3638,.T.);
#5405=EDGE_CURVE('',#4322,#4321,#982,.T.);
#5406=EDGE_CURVE('',#4322,#4323,#3639,.T.);
#5407=EDGE_CURVE('',#4324,#4323,#983,.T.);
#5408=EDGE_CURVE('',#4325,#4324,#984,.T.);
#5409=EDGE_CURVE('',#4326,#4325,#985,.T.);
#5410=EDGE_CURVE('',#4326,#4327,#3640,.T.);
#5411=EDGE_CURVE('',#4328,#4327,#986,.T.);
#5412=EDGE_CURVE('',#4328,#4329,#3641,.T.);
#5413=EDGE_CURVE('',#4329,#4330,#3642,.T.);
#5414=EDGE_CURVE('',#4331,#4330,#987,.T.);
#5415=EDGE_CURVE('',#4331,#4332,#3643,.T.);
#5416=EDGE_CURVE('',#4332,#4333,#3644,.T.);
#5417=EDGE_CURVE('',#4334,#4333,#988,.T.);
#5418=EDGE_CURVE('',#4334,#4335,#3645,.T.);
#5419=EDGE_CURVE('',#4335,#4336,#3646,.T.);
#5420=EDGE_CURVE('',#4310,#4336,#989,.T.);
#5421=EDGE_CURVE('',#4308,#4337,#990,.T.);
#5422=EDGE_CURVE('',#4337,#4314,#3647,.F.);
#5423=EDGE_CURVE('',#4338,#4307,#991,.T.);
#5424=EDGE_CURVE('',#4337,#4338,#992,.T.);
#5425=EDGE_CURVE('',#4306,#4339,#993,.T.);
#5426=EDGE_CURVE('',#4339,#4338,#3648,.F.);
#5427=EDGE_CURVE('',#4340,#4340,#3649,.T.);
#5428=EDGE_CURVE('',#4340,#4329,#994,.T.);
#5429=EDGE_CURVE('',#4341,#4328,#55,.T.);
#5430=EDGE_CURVE('',#4342,#4341,#995,.T.);
#5431=EDGE_CURVE('',#4343,#4342,#56,.T.);
#5432=EDGE_CURVE('',#4344,#4343,#3650,.T.);
#5433=EDGE_CURVE('',#4345,#4344,#57,.T.);
#5434=EDGE_CURVE('',#4346,#4345,#996,.T.);
#5435=EDGE_CURVE('',#4330,#4346,#58,.T.);
#5436=EDGE_CURVE('',#4347,#4347,#3651,.T.);
#5437=EDGE_CURVE('',#4347,#4348,#997,.T.);
#5438=EDGE_CURVE('',#4348,#4348,#3652,.T.);
#5439=EDGE_CURVE('',#4349,#4349,#3653,.T.);
#5440=EDGE_CURVE('',#4349,#4350,#998,.T.);
#5441=EDGE_CURVE('',#4350,#4350,#3654,.T.);
#5442=EDGE_CURVE('',#4351,#4351,#3655,.T.);
#5443=EDGE_CURVE('',#4351,#4352,#999,.T.);
#5444=EDGE_CURVE('',#4353,#4352,#3656,.T.);
#5445=EDGE_CURVE('',#4354,#4353,#59,.T.);
#5446=EDGE_CURVE('',#4355,#4354,#1000,.T.);
#5447=EDGE_CURVE('',#4323,#4355,#60,.T.);
#5448=EDGE_CURVE('',#4356,#4322,#61,.T.);
#5449=EDGE_CURVE('',#4357,#4356,#1001,.T.);
#5450=EDGE_CURVE('',#4358,#4357,#62,.T.);
#5451=EDGE_CURVE('',#4352,#4358,#3657,.T.);
#5452=EDGE_CURVE('',#4359,#4359,#3658,.T.);
#5453=EDGE_CURVE('',#4359,#4360,#1002,.T.);
#5454=EDGE_CURVE('',#4360,#4360,#3659,.T.);
#5455=EDGE_CURVE('',#4361,#4361,#3660,.T.);
#5456=EDGE_CURVE('',#4361,#4362,#1003,.T.);
#5457=EDGE_CURVE('',#4363,#4362,#3661,.T.);
#5458=EDGE_CURVE('',#4364,#4363,#63,.T.);
#5459=EDGE_CURVE('',#4365,#4364,#1004,.T.);
#5460=EDGE_CURVE('',#4321,#4365,#64,.T.);
#5461=EDGE_CURVE('',#4366,#4320,#65,.T.);
#5462=EDGE_CURVE('',#4367,#4366,#1005,.T.);
#5463=EDGE_CURVE('',#4368,#4367,#66,.T.);
#5464=EDGE_CURVE('',#4362,#4368,#3662,.T.);
#5465=EDGE_CURVE('',#4369,#4369,#3663,.T.);
#5466=EDGE_CURVE('',#4369,#4370,#1006,.T.);
#5467=EDGE_CURVE('',#4370,#4370,#3664,.T.);
#5468=EDGE_CURVE('',#4371,#4371,#3665,.T.);
#5469=EDGE_CURVE('',#4371,#4372,#1007,.T.);
#5470=EDGE_CURVE('',#4373,#4372,#3666,.T.);
#5471=EDGE_CURVE('',#4374,#4373,#67,.T.);
#5472=EDGE_CURVE('',#4375,#4374,#1008,.T.);
#5473=EDGE_CURVE('',#4317,#4375,#68,.T.);
#5474=EDGE_CURVE('',#4376,#4316,#69,.T.);
#5475=EDGE_CURVE('',#4377,#4376,#1009,.T.);
#5476=EDGE_CURVE('',#4378,#4377,#70,.T.);
#5477=EDGE_CURVE('',#4372,#4378,#3667,.T.);
#5478=EDGE_CURVE('',#4379,#4379,#3668,.T.);
#5479=EDGE_CURVE('',#4379,#4380,#1010,.T.);
#5480=EDGE_CURVE('',#4380,#4380,#3669,.T.);
#5481=EDGE_CURVE('',#4381,#4381,#3670,.T.);
#5482=EDGE_CURVE('',#4381,#4332,#1011,.T.);
#5483=EDGE_CURVE('',#4382,#4331,#71,.T.);
#5484=EDGE_CURVE('',#4383,#4382,#1012,.T.);
#5485=EDGE_CURVE('',#4384,#4383,#72,.T.);
#5486=EDGE_CURVE('',#4385,#4384,#3671,.T.);
#5487=EDGE_CURVE('',#4386,#4385,#73,.T.);
#5488=EDGE_CURVE('',#4387,#4386,#1013,.T.);
#5489=EDGE_CURVE('',#4333,#4387,#74,.T.);
#5490=EDGE_CURVE('',#4388,#4388,#3672,.T.);
#5491=EDGE_CURVE('',#4388,#4389,#1014,.T.);
#5492=EDGE_CURVE('',#4389,#4389,#3673,.T.);
#5493=EDGE_CURVE('',#4390,#4390,#3674,.T.);
#5494=EDGE_CURVE('',#4390,#4391,#1015,.T.);
#5495=EDGE_CURVE('',#4392,#4391,#3675,.T.);
#5496=EDGE_CURVE('',#4393,#4392,#75,.T.);
#5497=EDGE_CURVE('',#4394,#4393,#1016,.T.);
#5498=EDGE_CURVE('',#4319,#4394,#76,.T.);
#5499=EDGE_CURVE('',#4395,#4318,#77,.T.);
#5500=EDGE_CURVE('',#4396,#4395,#1017,.T.);
#5501=EDGE_CURVE('',#4397,#4396,#78,.T.);
#5502=EDGE_CURVE('',#4391,#4397,#3676,.T.);
#5503=EDGE_CURVE('',#4398,#4398,#3677,.T.);
#5504=EDGE_CURVE('',#4398,#4399,#1018,.T.);
#5505=EDGE_CURVE('',#4400,#4399,#3678,.T.);
#5506=EDGE_CURVE('',#4401,#4400,#79,.T.);
#5507=EDGE_CURVE('',#4402,#4401,#1019,.T.);
#5508=EDGE_CURVE('',#4403,#4402,#80,.T.);
#5509=EDGE_CURVE('',#4404,#4403,#3679,.T.);
#5510=EDGE_CURVE('',#4405,#4404,#81,.T.);
#5511=EDGE_CURVE('',#4406,#4405,#1020,.T.);
#5512=EDGE_CURVE('',#4407,#4406,#82,.T.);
#5513=EDGE_CURVE('',#4408,#4407,#3680,.T.);
#5514=EDGE_CURVE('',#4409,#4408,#83,.T.);
#5515=EDGE_CURVE('',#4410,#4409,#273,.T.);
#5516=EDGE_CURVE('',#4411,#4410,#84,.T.);
#5517=EDGE_CURVE('',#4412,#4411,#3681,.T.);
#5518=EDGE_CURVE('',#4413,#4412,#85,.T.);
#5519=EDGE_CURVE('',#4414,#4413,#274,.T.);
#5520=EDGE_CURVE('',#4415,#4414,#86,.T.);
#5521=EDGE_CURVE('',#4399,#4415,#3682,.T.);
#5522=EDGE_CURVE('',#4416,#4416,#3683,.T.);
#5523=EDGE_CURVE('',#4416,#4417,#1021,.T.);
#5524=EDGE_CURVE('',#4418,#4417,#3684,.T.);
#5525=EDGE_CURVE('',#4419,#4418,#87,.T.);
#5526=EDGE_CURVE('',#4420,#4419,#1022,.T.);
#5527=EDGE_CURVE('',#4327,#4420,#88,.T.);
#5528=EDGE_CURVE('',#4421,#4326,#89,.T.);
#5529=EDGE_CURVE('',#4422,#4421,#1023,.T.);
#5530=EDGE_CURVE('',#4423,#4422,#90,.T.);
#5531=EDGE_CURVE('',#4417,#4423,#3685,.T.);
#5532=EDGE_CURVE('',#4424,#4424,#3686,.T.);
#5533=EDGE_CURVE('',#4424,#4425,#1024,.T.);
#5534=EDGE_CURVE('',#4426,#4425,#3687,.T.);
#5535=EDGE_CURVE('',#4427,#4426,#91,.T.);
#5536=EDGE_CURVE('',#4428,#4427,#1025,.T.);
#5537=EDGE_CURVE('',#4429,#4428,#92,.T.);
#5538=EDGE_CURVE('',#4430,#4429,#3688,.T.);
#5539=EDGE_CURVE('',#4431,#4430,#93,.T.);
#5540=EDGE_CURVE('',#4432,#4431,#1026,.T.);
#5541=EDGE_CURVE('',#4433,#4432,#94,.T.);
#5542=EDGE_CURVE('',#4434,#4433,#3689,.T.);
#5543=EDGE_CURVE('',#4435,#4434,#95,.T.);
#5544=EDGE_CURVE('',#4436,#4435,#275,.T.);
#5545=EDGE_CURVE('',#4437,#4436,#96,.T.);
#5546=EDGE_CURVE('',#4438,#4437,#3690,.T.);
#5547=EDGE_CURVE('',#4439,#4438,#97,.T.);
#5548=EDGE_CURVE('',#4440,#4439,#276,.T.);
#5549=EDGE_CURVE('',#4441,#4440,#98,.T.);
#5550=EDGE_CURVE('',#4425,#4441,#3691,.T.);
#5551=EDGE_CURVE('',#4442,#4442,#3692,.T.);
#5552=EDGE_CURVE('',#4442,#4443,#1027,.T.);
#5553=EDGE_CURVE('',#4444,#4443,#3693,.T.);
#5554=EDGE_CURVE('',#4445,#4444,#99,.T.);
#5555=EDGE_CURVE('',#4446,#4445,#1028,.T.);
#5556=EDGE_CURVE('',#4447,#4446,#100,.T.);
#5557=EDGE_CURVE('',#4448,#4447,#3694,.T.);
#5558=EDGE_CURVE('',#4449,#4448,#101,.T.);
#5559=EDGE_CURVE('',#4450,#4449,#1029,.T.);
#5560=EDGE_CURVE('',#4451,#4450,#102,.T.);
#5561=EDGE_CURVE('',#4452,#4451,#3695,.T.);
#5562=EDGE_CURVE('',#4453,#4452,#103,.T.);
#5563=EDGE_CURVE('',#4454,#4453,#277,.T.);
#5564=EDGE_CURVE('',#4455,#4454,#104,.T.);
#5565=EDGE_CURVE('',#4456,#4455,#3696,.T.);
#5566=EDGE_CURVE('',#4457,#4456,#105,.T.);
#5567=EDGE_CURVE('',#4458,#4457,#278,.T.);
#5568=EDGE_CURVE('',#4459,#4458,#106,.T.);
#5569=EDGE_CURVE('',#4443,#4459,#3697,.T.);
#5570=EDGE_CURVE('',#4460,#4460,#3698,.T.);
#5571=EDGE_CURVE('',#4460,#4461,#1030,.T.);
#5572=EDGE_CURVE('',#4462,#4461,#3699,.T.);
#5573=EDGE_CURVE('',#4463,#4462,#107,.T.);
#5574=EDGE_CURVE('',#4464,#4463,#1031,.T.);
#5575=EDGE_CURVE('',#4465,#4464,#108,.T.);
#5576=EDGE_CURVE('',#4466,#4465,#3700,.T.);
#5577=EDGE_CURVE('',#4467,#4466,#109,.T.);
#5578=EDGE_CURVE('',#4468,#4467,#1032,.T.);
#5579=EDGE_CURVE('',#4469,#4468,#110,.T.);
#5580=EDGE_CURVE('',#4470,#4469,#3701,.T.);
#5581=EDGE_CURVE('',#4471,#4470,#111,.T.);
#5582=EDGE_CURVE('',#4472,#4471,#279,.T.);
#5583=EDGE_CURVE('',#4473,#4472,#112,.T.);
#5584=EDGE_CURVE('',#4474,#4473,#3702,.T.);
#5585=EDGE_CURVE('',#4475,#4474,#113,.T.);
#5586=EDGE_CURVE('',#4476,#4475,#280,.T.);
#5587=EDGE_CURVE('',#4477,#4476,#114,.T.);
#5588=EDGE_CURVE('',#4461,#4477,#3703,.T.);
#5589=EDGE_CURVE('',#4478,#4478,#3704,.T.);
#5590=EDGE_CURVE('',#4478,#4479,#1033,.T.);
#5591=EDGE_CURVE('',#4479,#4479,#3705,.T.);
#5592=EDGE_CURVE('',#4480,#4480,#3706,.T.);
#5593=EDGE_CURVE('',#4480,#4335,#1034,.T.);
#5594=EDGE_CURVE('',#4481,#4334,#115,.T.);
#5595=EDGE_CURVE('',#4482,#4481,#1035,.T.);
#5596=EDGE_CURVE('',#4483,#4482,#116,.T.);
#5597=EDGE_CURVE('',#4484,#4483,#3707,.T.);
#5598=EDGE_CURVE('',#4485,#4484,#117,.T.);
#5599=EDGE_CURVE('',#4486,#4485,#1036,.T.);
#5600=EDGE_CURVE('',#4336,#4486,#118,.T.);
#5601=EDGE_CURVE('',#4375,#4395,#1037,.T.);
#5602=EDGE_CURVE('',#4315,#4487,#3708,.F.);
#5603=EDGE_CURVE('',#4487,#4376,#1038,.T.);
#5604=EDGE_CURVE('',#4394,#4366,#1039,.T.);
#5605=EDGE_CURVE('',#4355,#4488,#1040,.T.);
#5606=EDGE_CURVE('',#4488,#4324,#3709,.F.);
#5607=EDGE_CURVE('',#4365,#4356,#1041,.T.);
#5608=EDGE_CURVE('',#4489,#4354,#1042,.T.);
#5609=EDGE_CURVE('',#4488,#4489,#1043,.T.);
#5610=EDGE_CURVE('',#4396,#4374,#1044,.T.);
#5611=EDGE_CURVE('',#4490,#4487,#1045,.T.);
#5612=EDGE_CURVE('',#4377,#4490,#1046,.T.);
#5613=EDGE_CURVE('',#4367,#4393,#1047,.T.);
#5614=EDGE_CURVE('',#4373,#4397,#1048,.T.);
#5615=EDGE_CURVE('',#4490,#4491,#3710,.F.);
#5616=EDGE_CURVE('',#4491,#4378,#1049,.T.);
#5617=EDGE_CURVE('',#4392,#4368,#1050,.T.);
#5618=EDGE_CURVE('',#4353,#4492,#1051,.T.);
#5619=EDGE_CURVE('',#4492,#4489,#3711,.F.);
#5620=EDGE_CURVE('',#4466,#4493,#1052,.T.);
#5621=EDGE_CURVE('',#4493,#4494,#3712,.F.);
#5622=EDGE_CURVE('',#4494,#4467,#1053,.T.);
#5623=EDGE_CURVE('',#4448,#4465,#1054,.T.);
#5624=EDGE_CURVE('',#4464,#4449,#1055,.T.);
#5625=EDGE_CURVE('',#4428,#4495,#1056,.T.);
#5626=EDGE_CURVE('',#4495,#4496,#3713,.F.);
#5627=EDGE_CURVE('',#4496,#4429,#1057,.T.);
#5628=EDGE_CURVE('',#4402,#4431,#1058,.T.);
#5629=EDGE_CURVE('',#4430,#4403,#1059,.T.);
#5630=EDGE_CURVE('',#4404,#4447,#1060,.T.);
#5631=EDGE_CURVE('',#4446,#4405,#1061,.T.);
#5632=EDGE_CURVE('',#4497,#4494,#1062,.T.);
#5633=EDGE_CURVE('',#4468,#4497,#1063,.T.);
#5634=EDGE_CURVE('',#4450,#4463,#1064,.T.);
#5635=EDGE_CURVE('',#4498,#4427,#1065,.T.);
#5636=EDGE_CURVE('',#4495,#4498,#1066,.T.);
#5637=EDGE_CURVE('',#4432,#4401,#1067,.T.);
#5638=EDGE_CURVE('',#4406,#4445,#1068,.T.);
#5639=EDGE_CURVE('',#4472,#4499,#1069,.T.);
#5640=EDGE_CURVE('',#4499,#4500,#3714,.F.);
#5641=EDGE_CURVE('',#4500,#4473,#1070,.T.);
#5642=EDGE_CURVE('',#4454,#4475,#1071,.T.);
#5643=EDGE_CURVE('',#4474,#4455,#1072,.T.);
#5644=EDGE_CURVE('',#4438,#4501,#1073,.T.);
#5645=EDGE_CURVE('',#4501,#4502,#3715,.F.);
#5646=EDGE_CURVE('',#4502,#4439,#1074,.T.);
#5647=EDGE_CURVE('',#4412,#4437,#1075,.T.);
#5648=EDGE_CURVE('',#4436,#4413,#1076,.T.);
#5649=EDGE_CURVE('',#4497,#4503,#3716,.F.);
#5650=EDGE_CURVE('',#4503,#4469,#1077,.T.);
#5651=EDGE_CURVE('',#4462,#4451,#1078,.T.);
#5652=EDGE_CURVE('',#4426,#4504,#1079,.T.);
#5653=EDGE_CURVE('',#4504,#4498,#3717,.F.);
#5654=EDGE_CURVE('',#4400,#4433,#1080,.T.);
#5655=EDGE_CURVE('',#4444,#4407,#1081,.T.);
#5656=EDGE_CURVE('',#4505,#4471,#1082,.T.);
#5657=EDGE_CURVE('',#4499,#4505,#1083,.T.);
#5658=EDGE_CURVE('',#4476,#4453,#1084,.T.);
#5659=EDGE_CURVE('',#4506,#4502,#1085,.T.);
#5660=EDGE_CURVE('',#4440,#4506,#1086,.T.);
#5661=EDGE_CURVE('',#4414,#4435,#1087,.T.);
#5662=EDGE_CURVE('',#4507,#4441,#1088,.T.);
#5663=EDGE_CURVE('',#4504,#4507,#1089,.T.);
#5664=EDGE_CURVE('',#4508,#4503,#1090,.T.);
#5665=EDGE_CURVE('',#4470,#4508,#1091,.T.);
#5666=EDGE_CURVE('',#4452,#4477,#1092,.T.);
#5667=EDGE_CURVE('',#4434,#4415,#1093,.T.);
#5668=EDGE_CURVE('',#4508,#4505,#3718,.F.);
#5669=EDGE_CURVE('',#4506,#4507,#3719,.F.);
#5670=EDGE_CURVE('',#4484,#4313,#1094,.T.);
#5671=EDGE_CURVE('',#4385,#4483,#1095,.T.);
#5672=EDGE_CURVE('',#4344,#4384,#1096,.T.);
#5673=EDGE_CURVE('',#4418,#4343,#1097,.T.);
#5674=EDGE_CURVE('',#4509,#4423,#1098,.T.);
#5675=EDGE_CURVE('',#4510,#4509,#1099,.T.);
#5676=EDGE_CURVE('',#4511,#4510,#1100,.T.);
#5677=EDGE_CURVE('',#4339,#4511,#1101,.T.);
#5678=EDGE_CURVE('',#4312,#4485,#1102,.T.);
#5679=EDGE_CURVE('',#4422,#4512,#1103,.T.);
#5680=EDGE_CURVE('',#4512,#4509,#3720,.F.);
#5681=EDGE_CURVE('',#4482,#4386,#1104,.T.);
#5682=EDGE_CURVE('',#4342,#4419,#1105,.T.);
#5683=EDGE_CURVE('',#4383,#4345,#1106,.T.);
#5684=EDGE_CURVE('',#4513,#4421,#1107,.T.);
#5685=EDGE_CURVE('',#4512,#4513,#1108,.T.);
#5686=EDGE_CURVE('',#4486,#4311,#1109,.T.);
#5687=EDGE_CURVE('',#4420,#4341,#1110,.T.);
#5688=EDGE_CURVE('',#4387,#4481,#1111,.T.);
#5689=EDGE_CURVE('',#4325,#4513,#3721,.F.);
#5690=EDGE_CURVE('',#4363,#4358,#1112,.T.);
#5691=EDGE_CURVE('',#4493,#4491,#1113,.T.);
#5692=EDGE_CURVE('',#4492,#4496,#1114,.T.);
#5693=EDGE_CURVE('',#4456,#4411,#1115,.T.);
#5694=EDGE_CURVE('',#4514,#4500,#1116,.T.);
#5695=EDGE_CURVE('',#4515,#4514,#1117,.T.);
#5696=EDGE_CURVE('',#4501,#4515,#1118,.T.);
#5697=EDGE_CURVE('',#4516,#4506,#3722,.F.);
#5698=EDGE_CURVE('',#4507,#4516,#3723,.F.);
#5699=EDGE_CURVE('',#4517,#4508,#3724,.F.);
#5700=EDGE_CURVE('',#4505,#4517,#3725,.F.);
#5701=EDGE_CURVE('',#4518,#4504,#3726,.T.);
#5702=EDGE_CURVE('',#4518,#4519,#3727,.T.);
#5703=EDGE_CURVE('',#4498,#4519,#3728,.T.);
#5704=EDGE_CURVE('',#4516,#4518,#1119,.T.);
#5705=EDGE_CURVE('',#4520,#4521,#3729,.T.);
#5706=EDGE_CURVE('',#4502,#4521,#3730,.T.);
#5707=EDGE_CURVE('',#4520,#4501,#3731,.T.);
#5708=EDGE_CURVE('',#4522,#4497,#3732,.T.);
#5709=EDGE_CURVE('',#4522,#4523,#3733,.T.);
#5710=EDGE_CURVE('',#4503,#4523,#3734,.T.);
#5711=EDGE_CURVE('',#4524,#4525,#3735,.T.);
#5712=EDGE_CURVE('',#4500,#4525,#3736,.T.);
#5713=EDGE_CURVE('',#4524,#4499,#3737,.T.);
#5714=EDGE_CURVE('',#4517,#4524,#1120,.T.);
#5715=EDGE_CURVE('',#4526,#4495,#3738,.F.);
#5716=EDGE_CURVE('',#4496,#4526,#3739,.F.);
#5717=EDGE_CURVE('',#4519,#4526,#1121,.T.);
#5718=EDGE_CURVE('',#4527,#4528,#3740,.F.);
#5719=EDGE_CURVE('',#4515,#4527,#3741,.F.);
#5720=EDGE_CURVE('',#4528,#4515,#3742,.F.);
#5721=EDGE_CURVE('',#4527,#4520,#1122,.T.);
#5722=EDGE_CURVE('',#4529,#4493,#3743,.F.);
#5723=EDGE_CURVE('',#4494,#4529,#3744,.F.);
#5724=EDGE_CURVE('',#4514,#4530,#3745,.F.);
#5725=EDGE_CURVE('',#4531,#4514,#3746,.F.);
#5726=EDGE_CURVE('',#4530,#4531,#3747,.F.);
#5727=EDGE_CURVE('',#4525,#4531,#1123,.T.);
#5728=EDGE_CURVE('',#4532,#4492,#3748,.F.);
#5729=EDGE_CURVE('',#4489,#4532,#3749,.F.);
#5730=EDGE_CURVE('',#4526,#4532,#1124,.T.);
#5731=EDGE_CURVE('',#4533,#4534,#3750,.F.);
#5732=EDGE_CURVE('',#4535,#4533,#3751,.F.);
#5733=EDGE_CURVE('',#4534,#4535,#3752,.F.);
#5734=EDGE_CURVE('',#4533,#4527,#1125,.T.);
#5735=EDGE_CURVE('',#4528,#4535,#1126,.T.);
#5736=EDGE_CURVE('',#4536,#4490,#3753,.F.);
#5737=EDGE_CURVE('',#4491,#4536,#3754,.F.);
#5738=EDGE_CURVE('',#4537,#4538,#3755,.F.);
#5739=EDGE_CURVE('',#4539,#4537,#3756,.F.);
#5740=EDGE_CURVE('',#4538,#4539,#3757,.F.);
#5741=EDGE_CURVE('',#4537,#4530,#1127,.T.);
#5742=EDGE_CURVE('',#4531,#4539,#1128,.T.);
#5743=EDGE_CURVE('',#4540,#4488,#3758,.T.);
#5744=EDGE_CURVE('',#4540,#4541,#3759,.T.);
#5745=EDGE_CURVE('',#4324,#4541,#3760,.T.);
#5746=EDGE_CURVE('',#4532,#4540,#1129,.T.);
#5747=EDGE_CURVE('',#4542,#4543,#3761,.F.);
#5748=EDGE_CURVE('',#4544,#4542,#3762,.F.);
#5749=EDGE_CURVE('',#4543,#4544,#3763,.F.);
#5750=EDGE_CURVE('',#4545,#4315,#3764,.T.);
#5751=EDGE_CURVE('',#4545,#4546,#3765,.T.);
#5752=EDGE_CURVE('',#4487,#4546,#3766,.T.);
#5753=EDGE_CURVE('',#4547,#4548,#3767,.F.);
#5754=EDGE_CURVE('',#4549,#4547,#3768,.F.);
#5755=EDGE_CURVE('',#4548,#4549,#3769,.F.);
#5756=EDGE_CURVE('',#4550,#4325,#3770,.F.);
#5757=EDGE_CURVE('',#4513,#4550,#3771,.F.);
#5758=EDGE_CURVE('',#4541,#4550,#1130,.T.);
#5759=EDGE_CURVE('',#4551,#4552,#3772,.F.);
#5760=EDGE_CURVE('',#4510,#4551,#3773,.F.);
#5761=EDGE_CURVE('',#4552,#4510,#3774,.F.);
#5762=EDGE_CURVE('',#4553,#4337,#3775,.F.);
#5763=EDGE_CURVE('',#4314,#4553,#3776,.F.);
#5764=EDGE_CURVE('',#4554,#4555,#3777,.F.);
#5765=EDGE_CURVE('',#4511,#4554,#3778,.F.);
#5766=EDGE_CURVE('',#4555,#4511,#3779,.F.);
#5767=EDGE_CURVE('',#4556,#4512,#3780,.T.);
#5768=EDGE_CURVE('',#4556,#4557,#3781,.T.);
#5769=EDGE_CURVE('',#4509,#4557,#3782,.T.);
#5770=EDGE_CURVE('',#4550,#4556,#1131,.T.);
#5771=EDGE_CURVE('',#4557,#4552,#1132,.T.);
#5772=EDGE_CURVE('',#4558,#4339,#3783,.T.);
#5773=EDGE_CURVE('',#4558,#4559,#3784,.T.);
#5774=EDGE_CURVE('',#4338,#4559,#3785,.T.);
#5775=EDGE_CURVE('',#4554,#4558,#1133,.T.);
#5776=EDGE_CURVE('',#4559,#4553,#1134,.T.);
#5777=EDGE_CURVE('',#4551,#4555,#1135,.T.);
#5778=EDGE_CURVE('',#4547,#4554,#1136,.T.);
#5779=EDGE_CURVE('',#4555,#4549,#1137,.T.);
#5780=EDGE_CURVE('',#4553,#4545,#1138,.T.);
#5781=EDGE_CURVE('',#4346,#4382,#1139,.T.);
#5782=EDGE_CURVE('',#4542,#4551,#1140,.T.);
#5783=EDGE_CURVE('',#4552,#4544,#1141,.T.);
#5784=EDGE_CURVE('',#4543,#4548,#1142,.T.);
#5785=EDGE_CURVE('',#4549,#4542,#1143,.T.);
#5786=EDGE_CURVE('',#4548,#4538,#1144,.T.);
#5787=EDGE_CURVE('',#4539,#4547,#1145,.T.);
#5788=EDGE_CURVE('',#4546,#4536,#1146,.T.);
#5789=EDGE_CURVE('',#4534,#4543,#1147,.T.);
#5790=EDGE_CURVE('',#4544,#4533,#1148,.T.);
#5791=EDGE_CURVE('',#4538,#4534,#1149,.T.);
#5792=EDGE_CURVE('',#4535,#4537,#1150,.T.);
#5793=EDGE_CURVE('',#4536,#4529,#1151,.T.);
#5794=EDGE_CURVE('',#4357,#4364,#1152,.T.);
#5795=EDGE_CURVE('',#4530,#4528,#1153,.T.);
#5796=EDGE_CURVE('',#4529,#4522,#1154,.T.);
#5797=EDGE_CURVE('',#4410,#4457,#1155,.T.);
#5798=EDGE_CURVE('',#4523,#4517,#1156,.T.);
#5799=EDGE_CURVE('',#4521,#4516,#1157,.T.);
#5800=EDGE_CURVE('',#4408,#4459,#1158,.T.);
#5801=EDGE_CURVE('',#4458,#4409,#1159,.T.);
#5802=EDGE_CURVE('',#4560,#4561,#3786,.T.);
#5803=EDGE_CURVE('',#4561,#4562,#1160,.T.);
#5804=EDGE_CURVE('',#4562,#4563,#3787,.T.);
#5805=EDGE_CURVE('',#4563,#4560,#1161,.T.);
#5806=EDGE_CURVE('',#4564,#4565,#3788,.T.);
#5807=EDGE_CURVE('',#4565,#4563,#3789,.T.);
#5808=EDGE_CURVE('',#4562,#4564,#3790,.T.);
#5809=EDGE_CURVE('',#4566,#4567,#3791,.T.);
#5810=EDGE_CURVE('',#4567,#4565,#1162,.T.);
#5811=EDGE_CURVE('',#4564,#4566,#1163,.T.);
#5812=EDGE_CURVE('',#4560,#4567,#3792,.T.);
#5813=EDGE_CURVE('',#4566,#4561,#3793,.T.);
#5814=EDGE_CURVE('',#4568,#4562,#1164,.T.);
#5815=EDGE_CURVE('',#4569,#4568,#3794,.T.);
#5816=EDGE_CURVE('',#4569,#4564,#1165,.T.);
#5817=EDGE_CURVE('',#4570,#4561,#1166,.T.);
#5818=EDGE_CURVE('',#4568,#4570,#1167,.T.);
#5819=EDGE_CURVE('',#4571,#4572,#1168,.T.);
#5820=EDGE_CURVE('',#4573,#4571,#1169,.T.);
#5821=EDGE_CURVE('',#4574,#4573,#1170,.T.);
#5822=EDGE_CURVE('',#4572,#4574,#1171,.T.);
#5823=EDGE_CURVE('',#4573,#4575,#3795,.T.);
#5824=EDGE_CURVE('',#4576,#4573,#3796,.F.);
#5825=EDGE_CURVE('',#4577,#4576,#3797,.T.);
#5826=EDGE_CURVE('',#4577,#4575,#3798,.T.);
#5827=EDGE_CURVE('',#4578,#4579,#3799,.F.);
#5828=EDGE_CURVE('',#4580,#4578,#3800,.F.);
#5829=EDGE_CURVE('',#4579,#4580,#3801,.F.);
#5830=EDGE_CURVE('',#4581,#4582,#3802,.T.);
#5831=EDGE_CURVE('',#4583,#4582,#3803,.T.);
#5832=EDGE_CURVE('',#4571,#4583,#3804,.F.);
#5833=EDGE_CURVE('',#4581,#4571,#3805,.T.);
#5834=EDGE_CURVE('',#4584,#4583,#1172,.T.);
#5835=EDGE_CURVE('',#4582,#4585,#1173,.T.);
#5836=EDGE_CURVE('',#4585,#4584,#281,.T.);
#5837=EDGE_CURVE('',#4586,#4587,#3806,.F.);
#5838=EDGE_CURVE('',#4574,#4586,#3807,.F.);
#5839=EDGE_CURVE('',#4587,#4574,#3808,.F.);
#5840=EDGE_CURVE('',#4588,#4589,#3809,.F.);
#5841=EDGE_CURVE('',#4590,#4588,#3810,.F.);
#5842=EDGE_CURVE('',#4589,#4590,#3811,.F.);
#5843=EDGE_CURVE('',#4585,#4590,#1174,.T.);
#5844=EDGE_CURVE('',#4588,#4584,#1175,.T.);
#5845=EDGE_CURVE('',#4591,#4592,#3812,.F.);
#5846=EDGE_CURVE('',#4593,#4591,#3813,.F.);
#5847=EDGE_CURVE('',#4592,#4593,#3814,.F.);
#5848=EDGE_CURVE('',#4594,#4572,#3815,.F.);
#5849=EDGE_CURVE('',#4595,#4594,#3816,.F.);
#5850=EDGE_CURVE('',#4572,#4595,#3817,.F.);
#5851=EDGE_CURVE('',#4596,#4597,#3818,.F.);
#5852=EDGE_CURVE('',#4598,#4596,#3819,.F.);
#5853=EDGE_CURVE('',#4597,#4598,#3820,.F.);
#5854=EDGE_CURVE('',#4599,#4600,#3821,.F.);
#5855=EDGE_CURVE('',#4601,#4599,#3822,.F.);
#5856=EDGE_CURVE('',#4600,#4601,#3823,.F.);
#5857=EDGE_CURVE('',#4599,#4589,#1176,.T.);
#5858=EDGE_CURVE('',#4590,#4601,#1177,.T.);
#5859=EDGE_CURVE('',#4602,#4603,#3824,.F.);
#5860=EDGE_CURVE('',#4604,#4602,#3825,.F.);
#5861=EDGE_CURVE('',#4603,#4604,#3826,.F.);
#5862=EDGE_CURVE('',#4601,#4604,#1178,.T.);
#5863=EDGE_CURVE('',#4602,#4600,#1179,.T.);
#5864=EDGE_CURVE('',#4604,#4595,#1180,.T.);
#5865=EDGE_CURVE('',#4594,#4603,#1181,.T.);
#5866=EDGE_CURVE('',#4596,#4602,#1182,.T.);
#5867=EDGE_CURVE('',#4603,#4598,#1183,.T.);
#5868=EDGE_CURVE('',#4591,#4599,#1184,.T.);
#5869=EDGE_CURVE('',#4600,#4593,#1185,.T.);
#5870=EDGE_CURVE('',#4587,#4597,#1186,.T.);
#5871=EDGE_CURVE('',#4598,#4586,#1187,.T.);
#5872=EDGE_CURVE('',#4597,#4592,#1188,.T.);
#5873=EDGE_CURVE('',#4593,#4596,#1189,.T.);
#5874=EDGE_CURVE('',#4595,#4581,#1190,.T.);
#5875=EDGE_CURVE('',#4586,#4594,#1191,.T.);
#5876=EDGE_CURVE('',#4592,#4579,#1192,.T.);
#5877=EDGE_CURVE('',#4580,#4591,#1193,.T.);
#5878=EDGE_CURVE('',#4578,#4588,#1194,.T.);
#5879=EDGE_CURVE('',#4589,#4580,#1195,.T.);
#5880=EDGE_CURVE('',#4575,#4587,#1196,.T.);
#5881=EDGE_CURVE('',#4583,#4576,#1197,.T.);
#5882=EDGE_CURVE('',#4605,#4578,#1198,.T.);
#5883=EDGE_CURVE('',#4579,#4606,#1199,.T.);
#5884=EDGE_CURVE('',#4606,#4605,#282,.T.);
#5885=EDGE_CURVE('',#4606,#4577,#1200,.T.);
#5886=EDGE_CURVE('',#4576,#4605,#1201,.T.);
#5887=EDGE_CURVE('',#4584,#4605,#1202,.T.);
#5888=EDGE_CURVE('',#4607,#4608,#1203,.T.);
#5889=EDGE_CURVE('',#4609,#4607,#3827,.T.);
#5890=EDGE_CURVE('',#4610,#4609,#1204,.T.);
#5891=EDGE_CURVE('',#4608,#4610,#3828,.T.);
#5892=EDGE_CURVE('',#4608,#4568,#3829,.T.);
#5893=EDGE_CURVE('',#4570,#4607,#3830,.T.);
#5894=EDGE_CURVE('',#4611,#4609,#3831,.T.);
#5895=EDGE_CURVE('',#4570,#4611,#3832,.T.);
#5896=EDGE_CURVE('',#4569,#4610,#3833,.T.);
#5897=EDGE_CURVE('',#4611,#4569,#1205,.T.);
#5898=EDGE_CURVE('',#4611,#4566,#1206,.T.);
#5899=EDGE_CURVE('',#4612,#4612,#3834,.T.);
#5900=EDGE_CURVE('',#4613,#4613,#3835,.T.);
#5901=EDGE_CURVE('',#4614,#4614,#3836,.T.);
#5902=EDGE_CURVE('',#4614,#4615,#1207,.T.);
#5903=EDGE_CURVE('',#4615,#4615,#3837,.T.);
#5904=EDGE_CURVE('',#4615,#4616,#1208,.T.);
#5905=EDGE_CURVE('',#4616,#4616,#3838,.T.);
#5906=EDGE_CURVE('',#4616,#4612,#1209,.T.);
#5907=EDGE_CURVE('',#4613,#4617,#1210,.T.);
#5908=EDGE_CURVE('',#4617,#4617,#3839,.T.);
#5909=EDGE_CURVE('',#4618,#4619,#3840,.T.);
#5910=EDGE_CURVE('',#4620,#4618,#1211,.T.);
#5911=EDGE_CURVE('',#4621,#4620,#3841,.T.);
#5912=EDGE_CURVE('',#4619,#4621,#1212,.T.);
#5913=EDGE_CURVE('',#4622,#4623,#3842,.T.);
#5914=EDGE_CURVE('',#4621,#4622,#3843,.T.);
#5915=EDGE_CURVE('',#4623,#4620,#3844,.T.);
#5916=EDGE_CURVE('',#4624,#4625,#3845,.T.);
#5917=EDGE_CURVE('',#4622,#4624,#1213,.T.);
#5918=EDGE_CURVE('',#4625,#4623,#1214,.T.);
#5919=EDGE_CURVE('',#4624,#4619,#3846,.T.);
#5920=EDGE_CURVE('',#4618,#4625,#3847,.T.);
#5921=EDGE_CURVE('',#4626,#4622,#1215,.T.);
#5922=EDGE_CURVE('',#4626,#4627,#3848,.T.);
#5923=EDGE_CURVE('',#4627,#4621,#1216,.T.);
#5924=EDGE_CURVE('',#4627,#4628,#1217,.T.);
#5925=EDGE_CURVE('',#4628,#4619,#1218,.T.);
#5926=EDGE_CURVE('',#4629,#4630,#1219,.T.);
#5927=EDGE_CURVE('',#4630,#4631,#1220,.T.);
#5928=EDGE_CURVE('',#4631,#4632,#1221,.T.);
#5929=EDGE_CURVE('',#4632,#4629,#1222,.T.);
#5930=EDGE_CURVE('',#4632,#4633,#3849,.T.);
#5931=EDGE_CURVE('',#4634,#4633,#3850,.T.);
#5932=EDGE_CURVE('',#4634,#4635,#3851,.T.);
#5933=EDGE_CURVE('',#4635,#4632,#3852,.F.);
#5934=EDGE_CURVE('',#4636,#4637,#3853,.F.);
#5935=EDGE_CURVE('',#4637,#4638,#3854,.F.);
#5936=EDGE_CURVE('',#4638,#4636,#3855,.F.);
#5937=EDGE_CURVE('',#4639,#4640,#3856,.T.);
#5938=EDGE_CURVE('',#4639,#4629,#3857,.T.);
#5939=EDGE_CURVE('',#4629,#4641,#3858,.F.);
#5940=EDGE_CURVE('',#4641,#4640,#3859,.T.);
#5941=EDGE_CURVE('',#4642,#4641,#1223,.T.);
#5942=EDGE_CURVE('',#4643,#4642,#283,.T.);
#5943=EDGE_CURVE('',#4640,#4643,#1224,.T.);
#5944=EDGE_CURVE('',#4644,#4645,#3860,.F.);
#5945=EDGE_CURVE('',#4645,#4631,#3861,.F.);
#5946=EDGE_CURVE('',#4631,#4644,#3862,.F.);
#5947=EDGE_CURVE('',#4646,#4647,#3863,.F.);
#5948=EDGE_CURVE('',#4647,#4648,#3864,.F.);
#5949=EDGE_CURVE('',#4648,#4646,#3865,.F.);
#5950=EDGE_CURVE('',#4643,#4648,#1225,.T.);
#5951=EDGE_CURVE('',#4646,#4642,#1226,.T.);
#5952=EDGE_CURVE('',#4649,#4650,#3866,.F.);
#5953=EDGE_CURVE('',#4650,#4651,#3867,.F.);
#5954=EDGE_CURVE('',#4651,#4649,#3868,.F.);
#5955=EDGE_CURVE('',#4652,#4630,#3869,.F.);
#5956=EDGE_CURVE('',#4630,#4653,#3870,.F.);
#5957=EDGE_CURVE('',#4653,#4652,#3871,.F.);
#5958=EDGE_CURVE('',#4654,#4655,#3872,.F.);
#5959=EDGE_CURVE('',#4655,#4656,#3873,.F.);
#5960=EDGE_CURVE('',#4656,#4654,#3874,.F.);
#5961=EDGE_CURVE('',#4657,#4658,#3875,.F.);
#5962=EDGE_CURVE('',#4658,#4659,#3876,.F.);
#5963=EDGE_CURVE('',#4659,#4657,#3877,.F.);
#5964=EDGE_CURVE('',#4648,#4659,#1227,.T.);
#5965=EDGE_CURVE('',#4657,#4647,#1228,.T.);
#5966=EDGE_CURVE('',#4660,#4661,#3878,.F.);
#5967=EDGE_CURVE('',#4661,#4662,#3879,.F.);
#5968=EDGE_CURVE('',#4662,#4660,#3880,.F.);
#5969=EDGE_CURVE('',#4660,#4658,#1229,.T.);
#5970=EDGE_CURVE('',#4659,#4662,#1230,.T.);
#5971=EDGE_CURVE('',#4652,#4661,#1231,.T.);
#5972=EDGE_CURVE('',#4662,#4653,#1232,.T.);
#5973=EDGE_CURVE('',#4661,#4656,#1233,.T.);
#5974=EDGE_CURVE('',#4654,#4660,#1234,.T.);
#5975=EDGE_CURVE('',#4658,#4651,#1235,.T.);
#5976=EDGE_CURVE('',#4649,#4657,#1236,.T.);
#5977=EDGE_CURVE('',#4656,#4644,#1237,.T.);
#5978=EDGE_CURVE('',#4645,#4655,#1238,.T.);
#5979=EDGE_CURVE('',#4651,#4654,#1239,.T.);
#5980=EDGE_CURVE('',#4655,#4650,#1240,.T.);
#5981=EDGE_CURVE('',#4653,#4639,#1241,.T.);
#5982=EDGE_CURVE('',#4644,#4652,#1242,.T.);
#5983=EDGE_CURVE('',#4638,#4649,#1243,.T.);
#5984=EDGE_CURVE('',#4650,#4637,#1244,.T.);
#5985=EDGE_CURVE('',#4647,#4638,#1245,.T.);
#5986=EDGE_CURVE('',#4636,#4646,#1246,.T.);
#5987=EDGE_CURVE('',#4633,#4645,#1247,.T.);
#5988=EDGE_CURVE('',#4641,#4635,#1248,.T.);
#5989=EDGE_CURVE('',#4663,#4636,#1249,.T.);
#5990=EDGE_CURVE('',#4664,#4663,#284,.T.);
#5991=EDGE_CURVE('',#4637,#4664,#1250,.T.);
#5992=EDGE_CURVE('',#4664,#4634,#1251,.T.);
#5993=EDGE_CURVE('',#4635,#4663,#1252,.T.);
#5994=EDGE_CURVE('',#4642,#4663,#1253,.T.);
#5995=EDGE_CURVE('',#4665,#4666,#1254,.T.);
#5996=EDGE_CURVE('',#4666,#4667,#3881,.T.);
#5997=EDGE_CURVE('',#4667,#4668,#1255,.T.);
#5998=EDGE_CURVE('',#4668,#4665,#3882,.T.);
#5999=EDGE_CURVE('',#4666,#4627,#3883,.T.);
#6000=EDGE_CURVE('',#4628,#4665,#3884,.T.);
#6001=EDGE_CURVE('',#4669,#4668,#3885,.T.);
#6002=EDGE_CURVE('',#4628,#4669,#3886,.T.);
#6003=EDGE_CURVE('',#4626,#4667,#3887,.T.);
#6004=EDGE_CURVE('',#4669,#4626,#1256,.T.);
#6005=EDGE_CURVE('',#4669,#4624,#1257,.T.);
#6006=EDGE_CURVE('',#4670,#4671,#3888,.T.);
#6007=EDGE_CURVE('',#4671,#4672,#1258,.T.);
#6008=EDGE_CURVE('',#4672,#4673,#3889,.T.);
#6009=EDGE_CURVE('',#4673,#4670,#1259,.T.);
#6010=EDGE_CURVE('',#4674,#4675,#3890,.T.);
#6011=EDGE_CURVE('',#4675,#4673,#3891,.T.);
#6012=EDGE_CURVE('',#4672,#4674,#3892,.T.);
#6013=EDGE_CURVE('',#4676,#4677,#3893,.T.);
#6014=EDGE_CURVE('',#4677,#4675,#1260,.T.);
#6015=EDGE_CURVE('',#4674,#4676,#1261,.T.);
#6016=EDGE_CURVE('',#4670,#4677,#3894,.T.);
#6017=EDGE_CURVE('',#4676,#4671,#3895,.T.);
#6018=EDGE_CURVE('',#4678,#4672,#1262,.T.);
#6019=EDGE_CURVE('',#4679,#4678,#3896,.T.);
#6020=EDGE_CURVE('',#4679,#4674,#1263,.T.);
#6021=EDGE_CURVE('',#4680,#4671,#1264,.T.);
#6022=EDGE_CURVE('',#4678,#4680,#1265,.T.);
#6023=EDGE_CURVE('',#4681,#4682,#1266,.T.);
#6024=EDGE_CURVE('',#4683,#4681,#1267,.T.);
#6025=EDGE_CURVE('',#4684,#4683,#1268,.T.);
#6026=EDGE_CURVE('',#4682,#4684,#1269,.T.);
#6027=EDGE_CURVE('',#4683,#4685,#3897,.T.);
#6028=EDGE_CURVE('',#4686,#4683,#3898,.F.);
#6029=EDGE_CURVE('',#4687,#4686,#3899,.T.);
#6030=EDGE_CURVE('',#4687,#4685,#3900,.T.);
#6031=EDGE_CURVE('',#4688,#4689,#3901,.F.);
#6032=EDGE_CURVE('',#4690,#4688,#3902,.F.);
#6033=EDGE_CURVE('',#4689,#4690,#3903,.F.);
#6034=EDGE_CURVE('',#4691,#4692,#3904,.T.);
#6035=EDGE_CURVE('',#4693,#4692,#3905,.T.);
#6036=EDGE_CURVE('',#4681,#4693,#3906,.F.);
#6037=EDGE_CURVE('',#4691,#4681,#3907,.T.);
#6038=EDGE_CURVE('',#4694,#4693,#1270,.T.);
#6039=EDGE_CURVE('',#4692,#4695,#1271,.T.);
#6040=EDGE_CURVE('',#4695,#4694,#285,.T.);
#6041=EDGE_CURVE('',#4696,#4697,#3908,.F.);
#6042=EDGE_CURVE('',#4684,#4696,#3909,.F.);
#6043=EDGE_CURVE('',#4697,#4684,#3910,.F.);
#6044=EDGE_CURVE('',#4698,#4699,#3911,.F.);
#6045=EDGE_CURVE('',#4700,#4698,#3912,.F.);
#6046=EDGE_CURVE('',#4699,#4700,#3913,.F.);
#6047=EDGE_CURVE('',#4695,#4700,#1272,.T.);
#6048=EDGE_CURVE('',#4698,#4694,#1273,.T.);
#6049=EDGE_CURVE('',#4701,#4702,#3914,.F.);
#6050=EDGE_CURVE('',#4703,#4701,#3915,.F.);
#6051=EDGE_CURVE('',#4702,#4703,#3916,.F.);
#6052=EDGE_CURVE('',#4704,#4682,#3917,.F.);
#6053=EDGE_CURVE('',#4705,#4704,#3918,.F.);
#6054=EDGE_CURVE('',#4682,#4705,#3919,.F.);
#6055=EDGE_CURVE('',#4706,#4707,#3920,.F.);
#6056=EDGE_CURVE('',#4708,#4706,#3921,.F.);
#6057=EDGE_CURVE('',#4707,#4708,#3922,.F.);
#6058=EDGE_CURVE('',#4709,#4710,#3923,.F.);
#6059=EDGE_CURVE('',#4711,#4709,#3924,.F.);
#6060=EDGE_CURVE('',#4710,#4711,#3925,.F.);
#6061=EDGE_CURVE('',#4709,#4699,#1274,.T.);
#6062=EDGE_CURVE('',#4700,#4711,#1275,.T.);
#6063=EDGE_CURVE('',#4712,#4713,#3926,.F.);
#6064=EDGE_CURVE('',#4714,#4712,#3927,.F.);
#6065=EDGE_CURVE('',#4713,#4714,#3928,.F.);
#6066=EDGE_CURVE('',#4711,#4714,#1276,.T.);
#6067=EDGE_CURVE('',#4712,#4710,#1277,.T.);
#6068=EDGE_CURVE('',#4714,#4705,#1278,.T.);
#6069=EDGE_CURVE('',#4704,#4713,#1279,.T.);
#6070=EDGE_CURVE('',#4706,#4712,#1280,.T.);
#6071=EDGE_CURVE('',#4713,#4708,#1281,.T.);
#6072=EDGE_CURVE('',#4701,#4709,#1282,.T.);
#6073=EDGE_CURVE('',#4710,#4703,#1283,.T.);
#6074=EDGE_CURVE('',#4697,#4707,#1284,.T.);
#6075=EDGE_CURVE('',#4708,#4696,#1285,.T.);
#6076=EDGE_CURVE('',#4707,#4702,#1286,.T.);
#6077=EDGE_CURVE('',#4703,#4706,#1287,.T.);
#6078=EDGE_CURVE('',#4705,#4691,#1288,.T.);
#6079=EDGE_CURVE('',#4696,#4704,#1289,.T.);
#6080=EDGE_CURVE('',#4702,#4689,#1290,.T.);
#6081=EDGE_CURVE('',#4690,#4701,#1291,.T.);
#6082=EDGE_CURVE('',#4688,#4698,#1292,.T.);
#6083=EDGE_CURVE('',#4699,#4690,#1293,.T.);
#6084=EDGE_CURVE('',#4685,#4697,#1294,.T.);
#6085=EDGE_CURVE('',#4693,#4686,#1295,.T.);
#6086=EDGE_CURVE('',#4715,#4688,#1296,.T.);
#6087=EDGE_CURVE('',#4689,#4716,#1297,.T.);
#6088=EDGE_CURVE('',#4716,#4715,#286,.T.);
#6089=EDGE_CURVE('',#4716,#4687,#1298,.T.);
#6090=EDGE_CURVE('',#4686,#4715,#1299,.T.);
#6091=EDGE_CURVE('',#4694,#4715,#1300,.T.);
#6092=EDGE_CURVE('',#4717,#4718,#1301,.T.);
#6093=EDGE_CURVE('',#4719,#4717,#3929,.T.);
#6094=EDGE_CURVE('',#4720,#4719,#1302,.T.);
#6095=EDGE_CURVE('',#4718,#4720,#3930,.T.);
#6096=EDGE_CURVE('',#4718,#4678,#3931,.T.);
#6097=EDGE_CURVE('',#4680,#4717,#3932,.T.);
#6098=EDGE_CURVE('',#4721,#4719,#3933,.T.);
#6099=EDGE_CURVE('',#4680,#4721,#3934,.T.);
#6100=EDGE_CURVE('',#4679,#4720,#3935,.T.);
#6101=EDGE_CURVE('',#4721,#4679,#1303,.T.);
#6102=EDGE_CURVE('',#4721,#4676,#1304,.T.);
#6103=ORIENTED_EDGE('',*,*,#4722,.F.);
#6104=ORIENTED_EDGE('',*,*,#4723,.T.);
#6105=ORIENTED_EDGE('',*,*,#4724,.T.);
#6106=ORIENTED_EDGE('',*,*,#4725,.T.);
#6107=ORIENTED_EDGE('',*,*,#4726,.T.);
#6108=ORIENTED_EDGE('',*,*,#4725,.F.);
#6109=ORIENTED_EDGE('',*,*,#4726,.F.);
#6110=ORIENTED_EDGE('',*,*,#4727,.T.);
#6111=ORIENTED_EDGE('',*,*,#4728,.F.);
#6112=ORIENTED_EDGE('',*,*,#4727,.F.);
#6113=ORIENTED_EDGE('',*,*,#4724,.F.);
#6114=ORIENTED_EDGE('',*,*,#4728,.T.);
#6115=ORIENTED_EDGE('',*,*,#4729,.T.);
#6116=ORIENTED_EDGE('',*,*,#4722,.T.);
#6117=ORIENTED_EDGE('',*,*,#4729,.F.);
#6118=ORIENTED_EDGE('',*,*,#4723,.F.);
#6119=ORIENTED_EDGE('',*,*,#4730,.T.);
#6120=ORIENTED_EDGE('',*,*,#4731,.T.);
#6121=ORIENTED_EDGE('',*,*,#4730,.F.);
#6122=ORIENTED_EDGE('',*,*,#4731,.F.);
#6123=ORIENTED_EDGE('',*,*,#4732,.F.);
#6124=ORIENTED_EDGE('',*,*,#4733,.F.);
#6125=ORIENTED_EDGE('',*,*,#4734,.T.);
#6126=ORIENTED_EDGE('',*,*,#4735,.F.);
#6127=ORIENTED_EDGE('',*,*,#4736,.F.);
#6128=ORIENTED_EDGE('',*,*,#4737,.F.);
#6129=ORIENTED_EDGE('',*,*,#4738,.F.);
#6130=ORIENTED_EDGE('',*,*,#4739,.F.);
#6131=ORIENTED_EDGE('',*,*,#4740,.F.);
#6132=ORIENTED_EDGE('',*,*,#4741,.F.);
#6133=ORIENTED_EDGE('',*,*,#4742,.F.);
#6134=ORIENTED_EDGE('',*,*,#4743,.F.);
#6135=ORIENTED_EDGE('',*,*,#4742,.T.);
#6136=ORIENTED_EDGE('',*,*,#4744,.F.);
#6137=ORIENTED_EDGE('',*,*,#4734,.F.);
#6138=ORIENTED_EDGE('',*,*,#4745,.F.);
#6139=ORIENTED_EDGE('',*,*,#4738,.T.);
#6140=ORIENTED_EDGE('',*,*,#4746,.T.);
#6141=ORIENTED_EDGE('',*,*,#4747,.T.);
#6142=ORIENTED_EDGE('',*,*,#4748,.T.);
#6143=ORIENTED_EDGE('',*,*,#4732,.T.);
#6144=ORIENTED_EDGE('',*,*,#4749,.T.);
#6145=ORIENTED_EDGE('',*,*,#4750,.T.);
#6146=ORIENTED_EDGE('',*,*,#4751,.T.);
#6147=ORIENTED_EDGE('',*,*,#4739,.T.);
#6148=ORIENTED_EDGE('',*,*,#4748,.F.);
#6149=ORIENTED_EDGE('',*,*,#4752,.T.);
#6150=ORIENTED_EDGE('',*,*,#4753,.F.);
#6151=ORIENTED_EDGE('',*,*,#4737,.T.);
#6152=ORIENTED_EDGE('',*,*,#4754,.F.);
#6153=ORIENTED_EDGE('',*,*,#4755,.F.);
#6154=ORIENTED_EDGE('',*,*,#4749,.F.);
#6155=ORIENTED_EDGE('',*,*,#4740,.T.);
#6156=ORIENTED_EDGE('',*,*,#4753,.T.);
#6157=ORIENTED_EDGE('',*,*,#4756,.F.);
#6158=ORIENTED_EDGE('',*,*,#4757,.T.);
#6159=ORIENTED_EDGE('',*,*,#4736,.T.);
#6160=ORIENTED_EDGE('',*,*,#4758,.T.);
#6161=ORIENTED_EDGE('',*,*,#4759,.T.);
#6162=ORIENTED_EDGE('',*,*,#4754,.T.);
#6163=ORIENTED_EDGE('',*,*,#4735,.T.);
#6164=ORIENTED_EDGE('',*,*,#4744,.T.);
#6165=ORIENTED_EDGE('',*,*,#4741,.T.);
#6166=ORIENTED_EDGE('',*,*,#4757,.F.);
#6167=ORIENTED_EDGE('',*,*,#4760,.F.);
#6168=ORIENTED_EDGE('',*,*,#4761,.F.);
#6169=ORIENTED_EDGE('',*,*,#4762,.T.);
#6170=ORIENTED_EDGE('',*,*,#4763,.T.);
#6171=ORIENTED_EDGE('',*,*,#4764,.T.);
#6172=ORIENTED_EDGE('',*,*,#4765,.F.);
#6173=ORIENTED_EDGE('',*,*,#4766,.F.);
#6174=ORIENTED_EDGE('',*,*,#4767,.F.);
#6175=ORIENTED_EDGE('',*,*,#4768,.F.);
#6176=ORIENTED_EDGE('',*,*,#4769,.F.);
#6177=ORIENTED_EDGE('',*,*,#4770,.F.);
#6178=ORIENTED_EDGE('',*,*,#4771,.F.);
#6179=ORIENTED_EDGE('',*,*,#4772,.F.);
#6180=ORIENTED_EDGE('',*,*,#4773,.F.);
#6181=ORIENTED_EDGE('',*,*,#4774,.F.);
#6182=ORIENTED_EDGE('',*,*,#4775,.F.);
#6183=ORIENTED_EDGE('',*,*,#4776,.F.);
#6184=ORIENTED_EDGE('',*,*,#4777,.F.);
#6185=ORIENTED_EDGE('',*,*,#4778,.F.);
#6186=ORIENTED_EDGE('',*,*,#4758,.F.);
#6187=ORIENTED_EDGE('',*,*,#4779,.F.);
#6188=ORIENTED_EDGE('',*,*,#4764,.F.);
#6189=ORIENTED_EDGE('',*,*,#4780,.F.);
#6190=ORIENTED_EDGE('',*,*,#4781,.F.);
#6191=ORIENTED_EDGE('',*,*,#4782,.F.);
#6192=ORIENTED_EDGE('',*,*,#4783,.F.);
#6193=ORIENTED_EDGE('',*,*,#4784,.F.);
#6194=ORIENTED_EDGE('',*,*,#4785,.F.);
#6195=ORIENTED_EDGE('',*,*,#4786,.F.);
#6196=ORIENTED_EDGE('',*,*,#4787,.F.);
#6197=ORIENTED_EDGE('',*,*,#4788,.T.);
#6198=ORIENTED_EDGE('',*,*,#4762,.F.);
#6199=ORIENTED_EDGE('',*,*,#4788,.F.);
#6200=ORIENTED_EDGE('',*,*,#4789,.F.);
#6201=ORIENTED_EDGE('',*,*,#4780,.T.);
#6202=ORIENTED_EDGE('',*,*,#4763,.F.);
#6203=ORIENTED_EDGE('',*,*,#4779,.T.);
#6204=ORIENTED_EDGE('',*,*,#4790,.T.);
#6205=ORIENTED_EDGE('',*,*,#4791,.T.);
#6206=ORIENTED_EDGE('',*,*,#4765,.T.);
#6207=ORIENTED_EDGE('',*,*,#4733,.T.);
#6208=ORIENTED_EDGE('',*,*,#4751,.F.);
#6209=ORIENTED_EDGE('',*,*,#4792,.F.);
#6210=ORIENTED_EDGE('',*,*,#4793,.F.);
#6211=ORIENTED_EDGE('',*,*,#4794,.F.);
#6212=ORIENTED_EDGE('',*,*,#4795,.F.);
#6213=ORIENTED_EDGE('',*,*,#4796,.F.);
#6214=ORIENTED_EDGE('',*,*,#4797,.F.);
#6215=ORIENTED_EDGE('',*,*,#4798,.F.);
#6216=ORIENTED_EDGE('',*,*,#4799,.F.);
#6217=ORIENTED_EDGE('',*,*,#4800,.F.);
#6218=ORIENTED_EDGE('',*,*,#4801,.F.);
#6219=ORIENTED_EDGE('',*,*,#4802,.F.);
#6220=ORIENTED_EDGE('',*,*,#4803,.F.);
#6221=ORIENTED_EDGE('',*,*,#4804,.F.);
#6222=ORIENTED_EDGE('',*,*,#4805,.F.);
#6223=ORIENTED_EDGE('',*,*,#4781,.T.);
#6224=ORIENTED_EDGE('',*,*,#4789,.T.);
#6225=ORIENTED_EDGE('',*,*,#4787,.T.);
#6226=ORIENTED_EDGE('',*,*,#4806,.F.);
#6227=ORIENTED_EDGE('',*,*,#4807,.F.);
#6228=ORIENTED_EDGE('',*,*,#4746,.F.);
#6229=ORIENTED_EDGE('',*,*,#4743,.T.);
#6230=ORIENTED_EDGE('',*,*,#4745,.T.);
#6231=ORIENTED_EDGE('',*,*,#4783,.T.);
#6232=ORIENTED_EDGE('',*,*,#4808,.F.);
#6233=ORIENTED_EDGE('',*,*,#4809,.F.);
#6234=ORIENTED_EDGE('',*,*,#4790,.F.);
#6235=ORIENTED_EDGE('',*,*,#4786,.T.);
#6236=ORIENTED_EDGE('',*,*,#4810,.T.);
#6237=ORIENTED_EDGE('',*,*,#4811,.T.);
#6238=ORIENTED_EDGE('',*,*,#4806,.T.);
#6239=ORIENTED_EDGE('',*,*,#4776,.T.);
#6240=ORIENTED_EDGE('',*,*,#4812,.F.);
#6241=ORIENTED_EDGE('',*,*,#4813,.F.);
#6242=ORIENTED_EDGE('',*,*,#4814,.F.);
#6243=ORIENTED_EDGE('',*,*,#4794,.T.);
#6244=ORIENTED_EDGE('',*,*,#4815,.F.);
#6245=ORIENTED_EDGE('',*,*,#4816,.F.);
#6246=ORIENTED_EDGE('',*,*,#4817,.F.);
#6247=ORIENTED_EDGE('',*,*,#4818,.F.);
#6248=ORIENTED_EDGE('',*,*,#4819,.F.);
#6249=ORIENTED_EDGE('',*,*,#4820,.F.);
#6250=ORIENTED_EDGE('',*,*,#4821,.F.);
#6251=ORIENTED_EDGE('',*,*,#4822,.F.);
#6252=ORIENTED_EDGE('',*,*,#4823,.F.);
#6253=ORIENTED_EDGE('',*,*,#4822,.T.);
#6254=ORIENTED_EDGE('',*,*,#4777,.T.);
#6255=ORIENTED_EDGE('',*,*,#4814,.T.);
#6256=ORIENTED_EDGE('',*,*,#4824,.T.);
#6257=ORIENTED_EDGE('',*,*,#4825,.F.);
#6258=ORIENTED_EDGE('',*,*,#4826,.F.);
#6259=ORIENTED_EDGE('',*,*,#4827,.F.);
#6260=ORIENTED_EDGE('',*,*,#4826,.T.);
#6261=ORIENTED_EDGE('',*,*,#4795,.T.);
#6262=ORIENTED_EDGE('',*,*,#4817,.T.);
#6263=ORIENTED_EDGE('',*,*,#4828,.T.);
#6264=ORIENTED_EDGE('',*,*,#4827,.T.);
#6265=ORIENTED_EDGE('',*,*,#4829,.T.);
#6266=ORIENTED_EDGE('',*,*,#4820,.T.);
#6267=ORIENTED_EDGE('',*,*,#4830,.T.);
#6268=ORIENTED_EDGE('',*,*,#4831,.F.);
#6269=ORIENTED_EDGE('',*,*,#4832,.F.);
#6270=ORIENTED_EDGE('',*,*,#4833,.F.);
#6271=ORIENTED_EDGE('',*,*,#4832,.T.);
#6272=ORIENTED_EDGE('',*,*,#4834,.T.);
#6273=ORIENTED_EDGE('',*,*,#4823,.T.);
#6274=ORIENTED_EDGE('',*,*,#4835,.T.);
#6275=ORIENTED_EDGE('',*,*,#4815,.T.);
#6276=ORIENTED_EDGE('',*,*,#4793,.T.);
#6277=ORIENTED_EDGE('',*,*,#4833,.T.);
#6278=ORIENTED_EDGE('',*,*,#4836,.T.);
#6279=ORIENTED_EDGE('',*,*,#4773,.T.);
#6280=ORIENTED_EDGE('',*,*,#4837,.F.);
#6281=ORIENTED_EDGE('',*,*,#4838,.F.);
#6282=ORIENTED_EDGE('',*,*,#4839,.F.);
#6283=ORIENTED_EDGE('',*,*,#4840,.F.);
#6284=ORIENTED_EDGE('',*,*,#4759,.F.);
#6285=ORIENTED_EDGE('',*,*,#4841,.F.);
#6286=ORIENTED_EDGE('',*,*,#4797,.T.);
#6287=ORIENTED_EDGE('',*,*,#4842,.F.);
#6288=ORIENTED_EDGE('',*,*,#4843,.F.);
#6289=ORIENTED_EDGE('',*,*,#4844,.F.);
#6290=ORIENTED_EDGE('',*,*,#4842,.T.);
#6291=ORIENTED_EDGE('',*,*,#4796,.T.);
#6292=ORIENTED_EDGE('',*,*,#4825,.T.);
#6293=ORIENTED_EDGE('',*,*,#4845,.T.);
#6294=ORIENTED_EDGE('',*,*,#4843,.T.);
#6295=ORIENTED_EDGE('',*,*,#4846,.T.);
#6296=ORIENTED_EDGE('',*,*,#4838,.T.);
#6297=ORIENTED_EDGE('',*,*,#4847,.T.);
#6298=ORIENTED_EDGE('',*,*,#4848,.F.);
#6299=ORIENTED_EDGE('',*,*,#4750,.F.);
#6300=ORIENTED_EDGE('',*,*,#4849,.F.);
#6301=ORIENTED_EDGE('',*,*,#4771,.T.);
#6302=ORIENTED_EDGE('',*,*,#4850,.F.);
#6303=ORIENTED_EDGE('',*,*,#4851,.F.);
#6304=ORIENTED_EDGE('',*,*,#4852,.F.);
#6305=ORIENTED_EDGE('',*,*,#4799,.T.);
#6306=ORIENTED_EDGE('',*,*,#4853,.F.);
#6307=ORIENTED_EDGE('',*,*,#4854,.F.);
#6308=ORIENTED_EDGE('',*,*,#4855,.F.);
#6309=ORIENTED_EDGE('',*,*,#4853,.T.);
#6310=ORIENTED_EDGE('',*,*,#4798,.T.);
#6311=ORIENTED_EDGE('',*,*,#4844,.T.);
#6312=ORIENTED_EDGE('',*,*,#4856,.T.);
#6313=ORIENTED_EDGE('',*,*,#4854,.T.);
#6314=ORIENTED_EDGE('',*,*,#4857,.T.);
#6315=ORIENTED_EDGE('',*,*,#4851,.T.);
#6316=ORIENTED_EDGE('',*,*,#4858,.T.);
#6317=ORIENTED_EDGE('',*,*,#4859,.F.);
#6318=ORIENTED_EDGE('',*,*,#4860,.F.);
#6319=ORIENTED_EDGE('',*,*,#4861,.F.);
#6320=ORIENTED_EDGE('',*,*,#4862,.F.);
#6321=ORIENTED_EDGE('',*,*,#4863,.F.);
#6322=ORIENTED_EDGE('',*,*,#4864,.F.);
#6323=ORIENTED_EDGE('',*,*,#4865,.T.);
#6324=ORIENTED_EDGE('',*,*,#4863,.T.);
#6325=ORIENTED_EDGE('',*,*,#4760,.T.);
#6326=ORIENTED_EDGE('',*,*,#4756,.T.);
#6327=ORIENTED_EDGE('',*,*,#4866,.F.);
#6328=ORIENTED_EDGE('',*,*,#4867,.F.);
#6329=ORIENTED_EDGE('',*,*,#4868,.F.);
#6330=ORIENTED_EDGE('',*,*,#4867,.T.);
#6331=ORIENTED_EDGE('',*,*,#4800,.T.);
#6332=ORIENTED_EDGE('',*,*,#4855,.T.);
#6333=ORIENTED_EDGE('',*,*,#4869,.T.);
#6334=ORIENTED_EDGE('',*,*,#4868,.T.);
#6335=ORIENTED_EDGE('',*,*,#4870,.T.);
#6336=ORIENTED_EDGE('',*,*,#4861,.T.);
#6337=ORIENTED_EDGE('',*,*,#4871,.T.);
#6338=ORIENTED_EDGE('',*,*,#4811,.F.);
#6339=ORIENTED_EDGE('',*,*,#4872,.F.);
#6340=ORIENTED_EDGE('',*,*,#4873,.F.);
#6341=ORIENTED_EDGE('',*,*,#4872,.T.);
#6342=ORIENTED_EDGE('',*,*,#4874,.T.);
#6343=ORIENTED_EDGE('',*,*,#4864,.T.);
#6344=ORIENTED_EDGE('',*,*,#4875,.T.);
#6345=ORIENTED_EDGE('',*,*,#4807,.T.);
#6346=ORIENTED_EDGE('',*,*,#4873,.T.);
#6347=ORIENTED_EDGE('',*,*,#4876,.T.);
#6348=ORIENTED_EDGE('',*,*,#4747,.F.);
#6349=ORIENTED_EDGE('',*,*,#4768,.T.);
#6350=ORIENTED_EDGE('',*,*,#4877,.F.);
#6351=ORIENTED_EDGE('',*,*,#4878,.F.);
#6352=ORIENTED_EDGE('',*,*,#4879,.F.);
#6353=ORIENTED_EDGE('',*,*,#4880,.F.);
#6354=ORIENTED_EDGE('',*,*,#4791,.F.);
#6355=ORIENTED_EDGE('',*,*,#4881,.F.);
#6356=ORIENTED_EDGE('',*,*,#4784,.T.);
#6357=ORIENTED_EDGE('',*,*,#4761,.T.);
#6358=ORIENTED_EDGE('',*,*,#4862,.T.);
#6359=ORIENTED_EDGE('',*,*,#4882,.T.);
#6360=ORIENTED_EDGE('',*,*,#4802,.T.);
#6361=ORIENTED_EDGE('',*,*,#4883,.F.);
#6362=ORIENTED_EDGE('',*,*,#4884,.F.);
#6363=ORIENTED_EDGE('',*,*,#4885,.F.);
#6364=ORIENTED_EDGE('',*,*,#4886,.F.);
#6365=ORIENTED_EDGE('',*,*,#4887,.F.);
#6366=ORIENTED_EDGE('',*,*,#4888,.F.);
#6367=ORIENTED_EDGE('',*,*,#4782,.T.);
#6368=ORIENTED_EDGE('',*,*,#4805,.T.);
#6369=ORIENTED_EDGE('',*,*,#4887,.T.);
#6370=ORIENTED_EDGE('',*,*,#4808,.T.);
#6371=ORIENTED_EDGE('',*,*,#4889,.F.);
#6372=ORIENTED_EDGE('',*,*,#4890,.F.);
#6373=ORIENTED_EDGE('',*,*,#4891,.F.);
#6374=ORIENTED_EDGE('',*,*,#4877,.T.);
#6375=ORIENTED_EDGE('',*,*,#4767,.T.);
#6376=ORIENTED_EDGE('',*,*,#4890,.T.);
#6377=ORIENTED_EDGE('',*,*,#4892,.T.);
#6378=ORIENTED_EDGE('',*,*,#4880,.T.);
#6379=ORIENTED_EDGE('',*,*,#4893,.T.);
#6380=ORIENTED_EDGE('',*,*,#4891,.T.);
#6381=ORIENTED_EDGE('',*,*,#4766,.T.);
#6382=ORIENTED_EDGE('',*,*,#4894,.F.);
#6383=ORIENTED_EDGE('',*,*,#4895,.F.);
#6384=ORIENTED_EDGE('',*,*,#4896,.F.);
#6385=ORIENTED_EDGE('',*,*,#4889,.T.);
#6386=ORIENTED_EDGE('',*,*,#4897,.T.);
#6387=ORIENTED_EDGE('',*,*,#4895,.T.);
#6388=ORIENTED_EDGE('',*,*,#4898,.T.);
#6389=ORIENTED_EDGE('',*,*,#4896,.T.);
#6390=ORIENTED_EDGE('',*,*,#4899,.T.);
#6391=ORIENTED_EDGE('',*,*,#4888,.T.);
#6392=ORIENTED_EDGE('',*,*,#4804,.T.);
#6393=ORIENTED_EDGE('',*,*,#4894,.T.);
#6394=ORIENTED_EDGE('',*,*,#4803,.T.);
#6395=ORIENTED_EDGE('',*,*,#4885,.T.);
#6396=ORIENTED_EDGE('',*,*,#4900,.T.);
#6397=ORIENTED_EDGE('',*,*,#4886,.T.);
#6398=ORIENTED_EDGE('',*,*,#4901,.T.);
#6399=ORIENTED_EDGE('',*,*,#4881,.T.);
#6400=ORIENTED_EDGE('',*,*,#4809,.T.);
#6401=ORIENTED_EDGE('',*,*,#4883,.T.);
#6402=ORIENTED_EDGE('',*,*,#4801,.T.);
#6403=ORIENTED_EDGE('',*,*,#4866,.T.);
#6404=ORIENTED_EDGE('',*,*,#4902,.T.);
#6405=ORIENTED_EDGE('',*,*,#4884,.T.);
#6406=ORIENTED_EDGE('',*,*,#4903,.T.);
#6407=ORIENTED_EDGE('',*,*,#4878,.T.);
#6408=ORIENTED_EDGE('',*,*,#4904,.T.);
#6409=ORIENTED_EDGE('',*,*,#4860,.T.);
#6410=ORIENTED_EDGE('',*,*,#4769,.T.);
#6411=ORIENTED_EDGE('',*,*,#4879,.T.);
#6412=ORIENTED_EDGE('',*,*,#4905,.T.);
#6413=ORIENTED_EDGE('',*,*,#4850,.T.);
#6414=ORIENTED_EDGE('',*,*,#4770,.T.);
#6415=ORIENTED_EDGE('',*,*,#4859,.T.);
#6416=ORIENTED_EDGE('',*,*,#4906,.T.);
#6417=ORIENTED_EDGE('',*,*,#4837,.T.);
#6418=ORIENTED_EDGE('',*,*,#4772,.T.);
#6419=ORIENTED_EDGE('',*,*,#4852,.T.);
#6420=ORIENTED_EDGE('',*,*,#4907,.T.);
#6421=ORIENTED_EDGE('',*,*,#4840,.T.);
#6422=ORIENTED_EDGE('',*,*,#4908,.T.);
#6423=ORIENTED_EDGE('',*,*,#4849,.T.);
#6424=ORIENTED_EDGE('',*,*,#4755,.T.);
#6425=ORIENTED_EDGE('',*,*,#4848,.T.);
#6426=ORIENTED_EDGE('',*,*,#4909,.T.);
#6427=ORIENTED_EDGE('',*,*,#4831,.T.);
#6428=ORIENTED_EDGE('',*,*,#4792,.T.);
#6429=ORIENTED_EDGE('',*,*,#4821,.T.);
#6430=ORIENTED_EDGE('',*,*,#4910,.T.);
#6431=ORIENTED_EDGE('',*,*,#4841,.T.);
#6432=ORIENTED_EDGE('',*,*,#4778,.T.);
#6433=ORIENTED_EDGE('',*,*,#4819,.T.);
#6434=ORIENTED_EDGE('',*,*,#4774,.T.);
#6435=ORIENTED_EDGE('',*,*,#4839,.T.);
#6436=ORIENTED_EDGE('',*,*,#4911,.T.);
#6437=ORIENTED_EDGE('',*,*,#4812,.T.);
#6438=ORIENTED_EDGE('',*,*,#4775,.T.);
#6439=ORIENTED_EDGE('',*,*,#4818,.T.);
#6440=ORIENTED_EDGE('',*,*,#4912,.T.);
#6441=ORIENTED_EDGE('',*,*,#4816,.T.);
#6442=ORIENTED_EDGE('',*,*,#4913,.T.);
#6443=ORIENTED_EDGE('',*,*,#4813,.T.);
#6444=ORIENTED_EDGE('',*,*,#4914,.T.);
#6445=ORIENTED_EDGE('',*,*,#4876,.F.);
#6446=ORIENTED_EDGE('',*,*,#4875,.F.);
#6447=ORIENTED_EDGE('',*,*,#4865,.F.);
#6448=ORIENTED_EDGE('',*,*,#4752,.F.);
#6449=ORIENTED_EDGE('',*,*,#4824,.F.);
#6450=ORIENTED_EDGE('',*,*,#4913,.F.);
#6451=ORIENTED_EDGE('',*,*,#4836,.F.);
#6452=ORIENTED_EDGE('',*,*,#4835,.F.);
#6453=ORIENTED_EDGE('',*,*,#4828,.F.);
#6454=ORIENTED_EDGE('',*,*,#4914,.F.);
#6455=ORIENTED_EDGE('',*,*,#4912,.F.);
#6456=ORIENTED_EDGE('',*,*,#4829,.F.);
#6457=ORIENTED_EDGE('',*,*,#4830,.F.);
#6458=ORIENTED_EDGE('',*,*,#4911,.F.);
#6459=ORIENTED_EDGE('',*,*,#4846,.F.);
#6460=ORIENTED_EDGE('',*,*,#4845,.F.);
#6461=ORIENTED_EDGE('',*,*,#4847,.F.);
#6462=ORIENTED_EDGE('',*,*,#4907,.F.);
#6463=ORIENTED_EDGE('',*,*,#4857,.F.);
#6464=ORIENTED_EDGE('',*,*,#4856,.F.);
#6465=ORIENTED_EDGE('',*,*,#4858,.F.);
#6466=ORIENTED_EDGE('',*,*,#4906,.F.);
#6467=ORIENTED_EDGE('',*,*,#4870,.F.);
#6468=ORIENTED_EDGE('',*,*,#4869,.F.);
#6469=ORIENTED_EDGE('',*,*,#4871,.F.);
#6470=ORIENTED_EDGE('',*,*,#4905,.F.);
#6471=ORIENTED_EDGE('',*,*,#4903,.F.);
#6472=ORIENTED_EDGE('',*,*,#4902,.F.);
#6473=ORIENTED_EDGE('',*,*,#4785,.T.);
#6474=ORIENTED_EDGE('',*,*,#4882,.F.);
#6475=ORIENTED_EDGE('',*,*,#4874,.F.);
#6476=ORIENTED_EDGE('',*,*,#4810,.F.);
#6477=ORIENTED_EDGE('',*,*,#4892,.F.);
#6478=ORIENTED_EDGE('',*,*,#4898,.F.);
#6479=ORIENTED_EDGE('',*,*,#4900,.F.);
#6480=ORIENTED_EDGE('',*,*,#4904,.F.);
#6481=ORIENTED_EDGE('',*,*,#4893,.F.);
#6482=ORIENTED_EDGE('',*,*,#4901,.F.);
#6483=ORIENTED_EDGE('',*,*,#4899,.F.);
#6484=ORIENTED_EDGE('',*,*,#4897,.F.);
#6485=ORIENTED_EDGE('',*,*,#4908,.F.);
#6486=ORIENTED_EDGE('',*,*,#4910,.F.);
#6487=ORIENTED_EDGE('',*,*,#4834,.F.);
#6488=ORIENTED_EDGE('',*,*,#4909,.F.);
#6489=ORIENTED_EDGE('',*,*,#4915,.F.);
#6490=ORIENTED_EDGE('',*,*,#4916,.T.);
#6491=ORIENTED_EDGE('',*,*,#4917,.F.);
#6492=ORIENTED_EDGE('',*,*,#4916,.F.);
#6493=ORIENTED_EDGE('',*,*,#4918,.F.);
#6494=ORIENTED_EDGE('',*,*,#4919,.T.);
#6495=ORIENTED_EDGE('',*,*,#4920,.T.);
#6496=ORIENTED_EDGE('',*,*,#4919,.F.);
#6497=ORIENTED_EDGE('',*,*,#4920,.F.);
#6498=ORIENTED_EDGE('',*,*,#4921,.F.);
#6499=ORIENTED_EDGE('',*,*,#4922,.T.);
#6500=ORIENTED_EDGE('',*,*,#4923,.T.);
#6501=ORIENTED_EDGE('',*,*,#4922,.F.);
#6502=ORIENTED_EDGE('',*,*,#4923,.F.);
#6503=ORIENTED_EDGE('',*,*,#4924,.F.);
#6504=ORIENTED_EDGE('',*,*,#4925,.T.);
#6505=ORIENTED_EDGE('',*,*,#4926,.F.);
#6506=ORIENTED_EDGE('',*,*,#4925,.F.);
#6507=ORIENTED_EDGE('',*,*,#4927,.F.);
#6508=ORIENTED_EDGE('',*,*,#4928,.F.);
#6509=ORIENTED_EDGE('',*,*,#4929,.F.);
#6510=ORIENTED_EDGE('',*,*,#4930,.F.);
#6511=ORIENTED_EDGE('',*,*,#4931,.F.);
#6512=ORIENTED_EDGE('',*,*,#4932,.F.);
#6513=ORIENTED_EDGE('',*,*,#4933,.F.);
#6514=ORIENTED_EDGE('',*,*,#4934,.F.);
#6515=ORIENTED_EDGE('',*,*,#4935,.T.);
#6516=ORIENTED_EDGE('',*,*,#4936,.F.);
#6517=ORIENTED_EDGE('',*,*,#4934,.T.);
#6518=ORIENTED_EDGE('',*,*,#4937,.T.);
#6519=ORIENTED_EDGE('',*,*,#4929,.T.);
#6520=ORIENTED_EDGE('',*,*,#4938,.T.);
#6521=ORIENTED_EDGE('',*,*,#4939,.T.);
#6522=ORIENTED_EDGE('',*,*,#4940,.F.);
#6523=ORIENTED_EDGE('',*,*,#4941,.F.);
#6524=ORIENTED_EDGE('',*,*,#4942,.F.);
#6525=ORIENTED_EDGE('',*,*,#4943,.F.);
#6526=ORIENTED_EDGE('',*,*,#4944,.F.);
#6527=ORIENTED_EDGE('',*,*,#4945,.T.);
#6528=ORIENTED_EDGE('',*,*,#4946,.F.);
#6529=ORIENTED_EDGE('',*,*,#4947,.T.);
#6530=ORIENTED_EDGE('',*,*,#4948,.F.);
#6531=ORIENTED_EDGE('',*,*,#4949,.F.);
#6532=ORIENTED_EDGE('',*,*,#4950,.F.);
#6533=ORIENTED_EDGE('',*,*,#4950,.T.);
#6534=ORIENTED_EDGE('',*,*,#4951,.T.);
#6535=ORIENTED_EDGE('',*,*,#4931,.T.);
#6536=ORIENTED_EDGE('',*,*,#4952,.T.);
#6537=ORIENTED_EDGE('',*,*,#4953,.F.);
#6538=ORIENTED_EDGE('',*,*,#4954,.F.);
#6539=ORIENTED_EDGE('',*,*,#4955,.F.);
#6540=ORIENTED_EDGE('',*,*,#4954,.T.);
#6541=ORIENTED_EDGE('',*,*,#4956,.T.);
#6542=ORIENTED_EDGE('',*,*,#4936,.T.);
#6543=ORIENTED_EDGE('',*,*,#4957,.T.);
#6544=ORIENTED_EDGE('',*,*,#4958,.F.);
#6545=ORIENTED_EDGE('',*,*,#4959,.F.);
#6546=ORIENTED_EDGE('',*,*,#4960,.F.);
#6547=ORIENTED_EDGE('',*,*,#4959,.T.);
#6548=ORIENTED_EDGE('',*,*,#4961,.T.);
#6549=ORIENTED_EDGE('',*,*,#4942,.T.);
#6550=ORIENTED_EDGE('',*,*,#4962,.T.);
#6551=ORIENTED_EDGE('',*,*,#4963,.F.);
#6552=ORIENTED_EDGE('',*,*,#4964,.F.);
#6553=ORIENTED_EDGE('',*,*,#4965,.F.);
#6554=ORIENTED_EDGE('',*,*,#4966,.F.);
#6555=ORIENTED_EDGE('',*,*,#4967,.F.);
#6556=ORIENTED_EDGE('',*,*,#4968,.F.);
#6557=ORIENTED_EDGE('',*,*,#4948,.T.);
#6558=ORIENTED_EDGE('',*,*,#4969,.T.);
#6559=ORIENTED_EDGE('',*,*,#4967,.T.);
#6560=ORIENTED_EDGE('',*,*,#4970,.T.);
#6561=ORIENTED_EDGE('',*,*,#4971,.F.);
#6562=ORIENTED_EDGE('',*,*,#4972,.F.);
#6563=ORIENTED_EDGE('',*,*,#4973,.F.);
#6564=ORIENTED_EDGE('',*,*,#4972,.T.);
#6565=ORIENTED_EDGE('',*,*,#4974,.T.);
#6566=ORIENTED_EDGE('',*,*,#4955,.T.);
#6567=ORIENTED_EDGE('',*,*,#4975,.T.);
#6568=ORIENTED_EDGE('',*,*,#4976,.F.);
#6569=ORIENTED_EDGE('',*,*,#4977,.F.);
#6570=ORIENTED_EDGE('',*,*,#4978,.F.);
#6571=ORIENTED_EDGE('',*,*,#4977,.T.);
#6572=ORIENTED_EDGE('',*,*,#4979,.T.);
#6573=ORIENTED_EDGE('',*,*,#4958,.T.);
#6574=ORIENTED_EDGE('',*,*,#4980,.T.);
#6575=ORIENTED_EDGE('',*,*,#4981,.F.);
#6576=ORIENTED_EDGE('',*,*,#4982,.F.);
#6577=ORIENTED_EDGE('',*,*,#4983,.F.);
#6578=ORIENTED_EDGE('',*,*,#4984,.F.);
#6579=ORIENTED_EDGE('',*,*,#4985,.F.);
#6580=ORIENTED_EDGE('',*,*,#4986,.F.);
#6581=ORIENTED_EDGE('',*,*,#4985,.T.);
#6582=ORIENTED_EDGE('',*,*,#4987,.T.);
#6583=ORIENTED_EDGE('',*,*,#4968,.T.);
#6584=ORIENTED_EDGE('',*,*,#4988,.T.);
#6585=ORIENTED_EDGE('',*,*,#4989,.F.);
#6586=ORIENTED_EDGE('',*,*,#4990,.F.);
#6587=ORIENTED_EDGE('',*,*,#4991,.T.);
#6588=ORIENTED_EDGE('',*,*,#4992,.F.);
#6589=ORIENTED_EDGE('',*,*,#4990,.T.);
#6590=ORIENTED_EDGE('',*,*,#4993,.T.);
#6591=ORIENTED_EDGE('',*,*,#4973,.T.);
#6592=ORIENTED_EDGE('',*,*,#4994,.T.);
#6593=ORIENTED_EDGE('',*,*,#4995,.F.);
#6594=ORIENTED_EDGE('',*,*,#4996,.F.);
#6595=ORIENTED_EDGE('',*,*,#4997,.F.);
#6596=ORIENTED_EDGE('',*,*,#4998,.F.);
#6597=ORIENTED_EDGE('',*,*,#4999,.F.);
#6598=ORIENTED_EDGE('',*,*,#5000,.T.);
#6599=ORIENTED_EDGE('',*,*,#5001,.F.);
#6600=ORIENTED_EDGE('',*,*,#5002,.F.);
#6601=ORIENTED_EDGE('',*,*,#5003,.F.);
#6602=ORIENTED_EDGE('',*,*,#5004,.F.);
#6603=ORIENTED_EDGE('',*,*,#5005,.F.);
#6604=ORIENTED_EDGE('',*,*,#5006,.F.);
#6605=ORIENTED_EDGE('',*,*,#5007,.F.);
#6606=ORIENTED_EDGE('',*,*,#5006,.T.);
#6607=ORIENTED_EDGE('',*,*,#5008,.T.);
#6608=ORIENTED_EDGE('',*,*,#4992,.T.);
#6609=ORIENTED_EDGE('',*,*,#5009,.T.);
#6610=ORIENTED_EDGE('',*,*,#5010,.F.);
#6611=ORIENTED_EDGE('',*,*,#5011,.F.);
#6612=ORIENTED_EDGE('',*,*,#5012,.F.);
#6613=ORIENTED_EDGE('',*,*,#5013,.F.);
#6614=ORIENTED_EDGE('',*,*,#5014,.F.);
#6615=ORIENTED_EDGE('',*,*,#5015,.F.);
#6616=ORIENTED_EDGE('',*,*,#5016,.F.);
#6617=ORIENTED_EDGE('',*,*,#5017,.F.);
#6618=ORIENTED_EDGE('',*,*,#5018,.F.);
#6619=ORIENTED_EDGE('',*,*,#5019,.F.);
#6620=ORIENTED_EDGE('',*,*,#5020,.F.);
#6621=ORIENTED_EDGE('',*,*,#5021,.T.);
#6622=ORIENTED_EDGE('',*,*,#5022,.F.);
#6623=ORIENTED_EDGE('',*,*,#5020,.T.);
#6624=ORIENTED_EDGE('',*,*,#5023,.T.);
#6625=ORIENTED_EDGE('',*,*,#5007,.T.);
#6626=ORIENTED_EDGE('',*,*,#5024,.T.);
#6627=ORIENTED_EDGE('',*,*,#5022,.T.);
#6628=ORIENTED_EDGE('',*,*,#5025,.T.);
#6629=ORIENTED_EDGE('',*,*,#5012,.T.);
#6630=ORIENTED_EDGE('',*,*,#5026,.T.);
#6631=ORIENTED_EDGE('',*,*,#5027,.F.);
#6632=ORIENTED_EDGE('',*,*,#5028,.F.);
#6633=ORIENTED_EDGE('',*,*,#5029,.T.);
#6634=ORIENTED_EDGE('',*,*,#5030,.F.);
#6635=ORIENTED_EDGE('',*,*,#5017,.T.);
#6636=ORIENTED_EDGE('',*,*,#5031,.T.);
#6637=ORIENTED_EDGE('',*,*,#5028,.T.);
#6638=ORIENTED_EDGE('',*,*,#5032,.T.);
#6639=ORIENTED_EDGE('',*,*,#5014,.T.);
#6640=ORIENTED_EDGE('',*,*,#5033,.T.);
#6641=ORIENTED_EDGE('',*,*,#5030,.T.);
#6642=ORIENTED_EDGE('',*,*,#5034,.T.);
#6643=ORIENTED_EDGE('',*,*,#5019,.T.);
#6644=ORIENTED_EDGE('',*,*,#5035,.T.);
#6645=ORIENTED_EDGE('',*,*,#5027,.T.);
#6646=ORIENTED_EDGE('',*,*,#5036,.T.);
#6647=ORIENTED_EDGE('',*,*,#5011,.T.);
#6648=ORIENTED_EDGE('',*,*,#5037,.T.);
#6649=ORIENTED_EDGE('',*,*,#5018,.T.);
#6650=ORIENTED_EDGE('',*,*,#5038,.T.);
#6651=ORIENTED_EDGE('',*,*,#5003,.T.);
#6652=ORIENTED_EDGE('',*,*,#5039,.T.);
#6653=ORIENTED_EDGE('',*,*,#5016,.T.);
#6654=ORIENTED_EDGE('',*,*,#5040,.T.);
#6655=ORIENTED_EDGE('',*,*,#4999,.T.);
#6656=ORIENTED_EDGE('',*,*,#5041,.T.);
#6657=ORIENTED_EDGE('',*,*,#5015,.T.);
#6658=ORIENTED_EDGE('',*,*,#5042,.T.);
#6659=ORIENTED_EDGE('',*,*,#5013,.T.);
#6660=ORIENTED_EDGE('',*,*,#5043,.T.);
#6661=ORIENTED_EDGE('',*,*,#5005,.T.);
#6662=ORIENTED_EDGE('',*,*,#5044,.T.);
#6663=ORIENTED_EDGE('',*,*,#4996,.T.);
#6664=ORIENTED_EDGE('',*,*,#5045,.T.);
#6665=ORIENTED_EDGE('',*,*,#5010,.T.);
#6666=ORIENTED_EDGE('',*,*,#5046,.T.);
#6667=ORIENTED_EDGE('',*,*,#4995,.T.);
#6668=ORIENTED_EDGE('',*,*,#5047,.T.);
#6669=ORIENTED_EDGE('',*,*,#5004,.T.);
#6670=ORIENTED_EDGE('',*,*,#5048,.T.);
#6671=ORIENTED_EDGE('',*,*,#5002,.T.);
#6672=ORIENTED_EDGE('',*,*,#5049,.T.);
#6673=ORIENTED_EDGE('',*,*,#4986,.T.);
#6674=ORIENTED_EDGE('',*,*,#5050,.T.);
#6675=ORIENTED_EDGE('',*,*,#4982,.T.);
#6676=ORIENTED_EDGE('',*,*,#5051,.T.);
#6677=ORIENTED_EDGE('',*,*,#5001,.T.);
#6678=ORIENTED_EDGE('',*,*,#5052,.T.);
#6679=ORIENTED_EDGE('',*,*,#4998,.T.);
#6680=ORIENTED_EDGE('',*,*,#5053,.T.);
#6681=ORIENTED_EDGE('',*,*,#4989,.T.);
#6682=ORIENTED_EDGE('',*,*,#5054,.T.);
#6683=ORIENTED_EDGE('',*,*,#4976,.T.);
#6684=ORIENTED_EDGE('',*,*,#5055,.T.);
#6685=ORIENTED_EDGE('',*,*,#4997,.T.);
#6686=ORIENTED_EDGE('',*,*,#5056,.T.);
#6687=ORIENTED_EDGE('',*,*,#4984,.T.);
#6688=ORIENTED_EDGE('',*,*,#5057,.T.);
#6689=ORIENTED_EDGE('',*,*,#4978,.T.);
#6690=ORIENTED_EDGE('',*,*,#5058,.T.);
#6691=ORIENTED_EDGE('',*,*,#4964,.T.);
#6692=ORIENTED_EDGE('',*,*,#5059,.T.);
#6693=ORIENTED_EDGE('',*,*,#4983,.T.);
#6694=ORIENTED_EDGE('',*,*,#5060,.T.);
#6695=ORIENTED_EDGE('',*,*,#4981,.T.);
#6696=ORIENTED_EDGE('',*,*,#5061,.T.);
#6697=ORIENTED_EDGE('',*,*,#4971,.T.);
#6698=ORIENTED_EDGE('',*,*,#5062,.T.);
#6699=ORIENTED_EDGE('',*,*,#4966,.T.);
#6700=ORIENTED_EDGE('',*,*,#5063,.T.);
#6701=ORIENTED_EDGE('',*,*,#4960,.T.);
#6702=ORIENTED_EDGE('',*,*,#5064,.T.);
#6703=ORIENTED_EDGE('',*,*,#4944,.T.);
#6704=ORIENTED_EDGE('',*,*,#5065,.T.);
#6705=ORIENTED_EDGE('',*,*,#4965,.T.);
#6706=ORIENTED_EDGE('',*,*,#5066,.T.);
#6707=ORIENTED_EDGE('',*,*,#4963,.T.);
#6708=ORIENTED_EDGE('',*,*,#5067,.T.);
#6709=ORIENTED_EDGE('',*,*,#4953,.T.);
#6710=ORIENTED_EDGE('',*,*,#5068,.T.);
#6711=ORIENTED_EDGE('',*,*,#4949,.T.);
#6712=ORIENTED_EDGE('',*,*,#5069,.T.);
#6713=ORIENTED_EDGE('',*,*,#4941,.T.);
#6714=ORIENTED_EDGE('',*,*,#5070,.T.);
#6715=ORIENTED_EDGE('',*,*,#4930,.T.);
#6716=ORIENTED_EDGE('',*,*,#5071,.T.);
#6717=ORIENTED_EDGE('',*,*,#4946,.T.);
#6718=ORIENTED_EDGE('',*,*,#5072,.T.);
#6719=ORIENTED_EDGE('',*,*,#4943,.T.);
#6720=ORIENTED_EDGE('',*,*,#5073,.T.);
#6721=ORIENTED_EDGE('',*,*,#4933,.T.);
#6722=ORIENTED_EDGE('',*,*,#5074,.T.);
#6723=ORIENTED_EDGE('',*,*,#4928,.T.);
#6724=ORIENTED_EDGE('',*,*,#5075,.T.);
#6725=ORIENTED_EDGE('',*,*,#4940,.T.);
#6726=ORIENTED_EDGE('',*,*,#5076,.T.);
#6727=ORIENTED_EDGE('',*,*,#4932,.T.);
#6728=ORIENTED_EDGE('',*,*,#5077,.T.);
#6729=ORIENTED_EDGE('',*,*,#4927,.T.);
#6730=ORIENTED_EDGE('',*,*,#5078,.T.);
#6731=ORIENTED_EDGE('',*,*,#4947,.F.);
#6732=ORIENTED_EDGE('',*,*,#4952,.F.);
#6733=ORIENTED_EDGE('',*,*,#5072,.F.);
#6734=ORIENTED_EDGE('',*,*,#4945,.F.);
#6735=ORIENTED_EDGE('',*,*,#5066,.F.);
#6736=ORIENTED_EDGE('',*,*,#5060,.F.);
#6737=ORIENTED_EDGE('',*,*,#5052,.F.);
#6738=ORIENTED_EDGE('',*,*,#5000,.F.);
#6739=ORIENTED_EDGE('',*,*,#5042,.F.);
#6740=ORIENTED_EDGE('',*,*,#5034,.F.);
#6741=ORIENTED_EDGE('',*,*,#5029,.F.);
#6742=ORIENTED_EDGE('',*,*,#5031,.F.);
#6743=ORIENTED_EDGE('',*,*,#5039,.F.);
#6744=ORIENTED_EDGE('',*,*,#5050,.F.);
#6745=ORIENTED_EDGE('',*,*,#4988,.F.);
#6746=ORIENTED_EDGE('',*,*,#4969,.F.);
#6747=ORIENTED_EDGE('',*,*,#4951,.F.);
#6748=ORIENTED_EDGE('',*,*,#5070,.F.);
#6749=ORIENTED_EDGE('',*,*,#5075,.F.);
#6750=ORIENTED_EDGE('',*,*,#5077,.F.);
#6751=ORIENTED_EDGE('',*,*,#4970,.F.);
#6752=ORIENTED_EDGE('',*,*,#5064,.F.);
#6753=ORIENTED_EDGE('',*,*,#4962,.F.);
#6754=ORIENTED_EDGE('',*,*,#5069,.F.);
#6755=ORIENTED_EDGE('',*,*,#4917,.T.);
#6756=ORIENTED_EDGE('',*,*,#4926,.T.);
#6757=ORIENTED_EDGE('',*,*,#4987,.F.);
#6758=ORIENTED_EDGE('',*,*,#5058,.F.);
#6759=ORIENTED_EDGE('',*,*,#4980,.F.);
#6760=ORIENTED_EDGE('',*,*,#5063,.F.);
#6761=ORIENTED_EDGE('',*,*,#5032,.F.);
#6762=ORIENTED_EDGE('',*,*,#5035,.F.);
#6763=ORIENTED_EDGE('',*,*,#5026,.F.);
#6764=ORIENTED_EDGE('',*,*,#5038,.F.);
#6765=ORIENTED_EDGE('',*,*,#5033,.F.);
#6766=ORIENTED_EDGE('',*,*,#5044,.F.);
#6767=ORIENTED_EDGE('',*,*,#5023,.F.);
#6768=ORIENTED_EDGE('',*,*,#5036,.F.);
#6769=ORIENTED_EDGE('',*,*,#5037,.F.);
#6770=ORIENTED_EDGE('',*,*,#5045,.F.);
#6771=ORIENTED_EDGE('',*,*,#5048,.F.);
#6772=ORIENTED_EDGE('',*,*,#5040,.F.);
#6773=ORIENTED_EDGE('',*,*,#5041,.F.);
#6774=ORIENTED_EDGE('',*,*,#5054,.F.);
#6775=ORIENTED_EDGE('',*,*,#5008,.F.);
#6776=ORIENTED_EDGE('',*,*,#5043,.F.);
#6777=ORIENTED_EDGE('',*,*,#5047,.F.);
#6778=ORIENTED_EDGE('',*,*,#5055,.F.);
#6779=ORIENTED_EDGE('',*,*,#5057,.F.);
#6780=ORIENTED_EDGE('',*,*,#5049,.F.);
#6781=ORIENTED_EDGE('',*,*,#4915,.T.);
#6782=ORIENTED_EDGE('',*,*,#4918,.T.);
#6783=ORIENTED_EDGE('',*,*,#4921,.T.);
#6784=ORIENTED_EDGE('',*,*,#4924,.T.);
#6785=ORIENTED_EDGE('',*,*,#5051,.F.);
#6786=ORIENTED_EDGE('',*,*,#5062,.F.);
#6787=ORIENTED_EDGE('',*,*,#4993,.F.);
#6788=ORIENTED_EDGE('',*,*,#5053,.F.);
#6789=ORIENTED_EDGE('',*,*,#5059,.F.);
#6790=ORIENTED_EDGE('',*,*,#5068,.F.);
#6791=ORIENTED_EDGE('',*,*,#4974,.F.);
#6792=ORIENTED_EDGE('',*,*,#5061,.F.);
#6793=ORIENTED_EDGE('',*,*,#5065,.F.);
#6794=ORIENTED_EDGE('',*,*,#5074,.F.);
#6795=ORIENTED_EDGE('',*,*,#4956,.F.);
#6796=ORIENTED_EDGE('',*,*,#5067,.F.);
#6797=ORIENTED_EDGE('',*,*,#5071,.F.);
#6798=ORIENTED_EDGE('',*,*,#5078,.F.);
#6799=ORIENTED_EDGE('',*,*,#4937,.F.);
#6800=ORIENTED_EDGE('',*,*,#5073,.F.);
#6801=ORIENTED_EDGE('',*,*,#4939,.F.);
#6802=ORIENTED_EDGE('',*,*,#4961,.F.);
#6803=ORIENTED_EDGE('',*,*,#4979,.F.);
#6804=ORIENTED_EDGE('',*,*,#5056,.F.);
#6805=ORIENTED_EDGE('',*,*,#5046,.F.);
#6806=ORIENTED_EDGE('',*,*,#5025,.F.);
#6807=ORIENTED_EDGE('',*,*,#5021,.F.);
#6808=ORIENTED_EDGE('',*,*,#5024,.F.);
#6809=ORIENTED_EDGE('',*,*,#5009,.F.);
#6810=ORIENTED_EDGE('',*,*,#4991,.F.);
#6811=ORIENTED_EDGE('',*,*,#4994,.F.);
#6812=ORIENTED_EDGE('',*,*,#4975,.F.);
#6813=ORIENTED_EDGE('',*,*,#4957,.F.);
#6814=ORIENTED_EDGE('',*,*,#4935,.F.);
#6815=ORIENTED_EDGE('',*,*,#4938,.F.);
#6816=ORIENTED_EDGE('',*,*,#5076,.F.);
#6817=ORIENTED_EDGE('',*,*,#5079,.F.);
#6818=ORIENTED_EDGE('',*,*,#5080,.T.);
#6819=ORIENTED_EDGE('',*,*,#5081,.F.);
#6820=ORIENTED_EDGE('',*,*,#5080,.F.);
#6821=ORIENTED_EDGE('',*,*,#5081,.T.);
#6822=ORIENTED_EDGE('',*,*,#5082,.F.);
#6823=ORIENTED_EDGE('',*,*,#5083,.T.);
#6824=ORIENTED_EDGE('',*,*,#5084,.F.);
#6825=ORIENTED_EDGE('',*,*,#5083,.F.);
#6826=ORIENTED_EDGE('',*,*,#5084,.T.);
#6827=ORIENTED_EDGE('',*,*,#5085,.F.);
#6828=ORIENTED_EDGE('',*,*,#5086,.T.);
#6829=ORIENTED_EDGE('',*,*,#5087,.F.);
#6830=ORIENTED_EDGE('',*,*,#5086,.F.);
#6831=ORIENTED_EDGE('',*,*,#5087,.T.);
#6832=ORIENTED_EDGE('',*,*,#5088,.F.);
#6833=ORIENTED_EDGE('',*,*,#5089,.T.);
#6834=ORIENTED_EDGE('',*,*,#5090,.F.);
#6835=ORIENTED_EDGE('',*,*,#5089,.F.);
#6836=ORIENTED_EDGE('',*,*,#5090,.T.);
#6837=ORIENTED_EDGE('',*,*,#5091,.F.);
#6838=ORIENTED_EDGE('',*,*,#5092,.T.);
#6839=ORIENTED_EDGE('',*,*,#5093,.T.);
#6840=ORIENTED_EDGE('',*,*,#5092,.F.);
#6841=ORIENTED_EDGE('',*,*,#5093,.F.);
#6842=ORIENTED_EDGE('',*,*,#5094,.F.);
#6843=ORIENTED_EDGE('',*,*,#5095,.T.);
#6844=ORIENTED_EDGE('',*,*,#5096,.T.);
#6845=ORIENTED_EDGE('',*,*,#5095,.F.);
#6846=ORIENTED_EDGE('',*,*,#5096,.F.);
#6847=ORIENTED_EDGE('',*,*,#5097,.F.);
#6848=ORIENTED_EDGE('',*,*,#5098,.T.);
#6849=ORIENTED_EDGE('',*,*,#5099,.T.);
#6850=ORIENTED_EDGE('',*,*,#5098,.F.);
#6851=ORIENTED_EDGE('',*,*,#5099,.F.);
#6852=ORIENTED_EDGE('',*,*,#5100,.F.);
#6853=ORIENTED_EDGE('',*,*,#5101,.T.);
#6854=ORIENTED_EDGE('',*,*,#5102,.T.);
#6855=ORIENTED_EDGE('',*,*,#5101,.F.);
#6856=ORIENTED_EDGE('',*,*,#5102,.F.);
#6857=ORIENTED_EDGE('',*,*,#5103,.F.);
#6858=ORIENTED_EDGE('',*,*,#5104,.F.);
#6859=ORIENTED_EDGE('',*,*,#5105,.T.);
#6860=ORIENTED_EDGE('',*,*,#5106,.F.);
#6861=ORIENTED_EDGE('',*,*,#5107,.F.);
#6862=ORIENTED_EDGE('',*,*,#5108,.F.);
#6863=ORIENTED_EDGE('',*,*,#5109,.F.);
#6864=ORIENTED_EDGE('',*,*,#5110,.F.);
#6865=ORIENTED_EDGE('',*,*,#5111,.F.);
#6866=ORIENTED_EDGE('',*,*,#5112,.F.);
#6867=ORIENTED_EDGE('',*,*,#5113,.F.);
#6868=ORIENTED_EDGE('',*,*,#5114,.F.);
#6869=ORIENTED_EDGE('',*,*,#5113,.T.);
#6870=ORIENTED_EDGE('',*,*,#5115,.F.);
#6871=ORIENTED_EDGE('',*,*,#5105,.F.);
#6872=ORIENTED_EDGE('',*,*,#5116,.F.);
#6873=ORIENTED_EDGE('',*,*,#5109,.T.);
#6874=ORIENTED_EDGE('',*,*,#5117,.T.);
#6875=ORIENTED_EDGE('',*,*,#5118,.T.);
#6876=ORIENTED_EDGE('',*,*,#5119,.T.);
#6877=ORIENTED_EDGE('',*,*,#5103,.T.);
#6878=ORIENTED_EDGE('',*,*,#5120,.T.);
#6879=ORIENTED_EDGE('',*,*,#5121,.T.);
#6880=ORIENTED_EDGE('',*,*,#5122,.T.);
#6881=ORIENTED_EDGE('',*,*,#5110,.T.);
#6882=ORIENTED_EDGE('',*,*,#5119,.F.);
#6883=ORIENTED_EDGE('',*,*,#5123,.T.);
#6884=ORIENTED_EDGE('',*,*,#5124,.F.);
#6885=ORIENTED_EDGE('',*,*,#5108,.T.);
#6886=ORIENTED_EDGE('',*,*,#5125,.F.);
#6887=ORIENTED_EDGE('',*,*,#5126,.F.);
#6888=ORIENTED_EDGE('',*,*,#5120,.F.);
#6889=ORIENTED_EDGE('',*,*,#5091,.T.);
#6890=ORIENTED_EDGE('',*,*,#5094,.T.);
#6891=ORIENTED_EDGE('',*,*,#5097,.T.);
#6892=ORIENTED_EDGE('',*,*,#5100,.T.);
#6893=ORIENTED_EDGE('',*,*,#5111,.T.);
#6894=ORIENTED_EDGE('',*,*,#5124,.T.);
#6895=ORIENTED_EDGE('',*,*,#5127,.F.);
#6896=ORIENTED_EDGE('',*,*,#5128,.T.);
#6897=ORIENTED_EDGE('',*,*,#5107,.T.);
#6898=ORIENTED_EDGE('',*,*,#5129,.T.);
#6899=ORIENTED_EDGE('',*,*,#5130,.T.);
#6900=ORIENTED_EDGE('',*,*,#5125,.T.);
#6901=ORIENTED_EDGE('',*,*,#5106,.T.);
#6902=ORIENTED_EDGE('',*,*,#5115,.T.);
#6903=ORIENTED_EDGE('',*,*,#5112,.T.);
#6904=ORIENTED_EDGE('',*,*,#5128,.F.);
#6905=ORIENTED_EDGE('',*,*,#5131,.F.);
#6906=ORIENTED_EDGE('',*,*,#5132,.F.);
#6907=ORIENTED_EDGE('',*,*,#5133,.T.);
#6908=ORIENTED_EDGE('',*,*,#5134,.T.);
#6909=ORIENTED_EDGE('',*,*,#5135,.T.);
#6910=ORIENTED_EDGE('',*,*,#5136,.F.);
#6911=ORIENTED_EDGE('',*,*,#5137,.F.);
#6912=ORIENTED_EDGE('',*,*,#5138,.F.);
#6913=ORIENTED_EDGE('',*,*,#5139,.F.);
#6914=ORIENTED_EDGE('',*,*,#5140,.F.);
#6915=ORIENTED_EDGE('',*,*,#5141,.F.);
#6916=ORIENTED_EDGE('',*,*,#5142,.F.);
#6917=ORIENTED_EDGE('',*,*,#5143,.F.);
#6918=ORIENTED_EDGE('',*,*,#5144,.F.);
#6919=ORIENTED_EDGE('',*,*,#5145,.F.);
#6920=ORIENTED_EDGE('',*,*,#5146,.F.);
#6921=ORIENTED_EDGE('',*,*,#5147,.F.);
#6922=ORIENTED_EDGE('',*,*,#5148,.F.);
#6923=ORIENTED_EDGE('',*,*,#5149,.F.);
#6924=ORIENTED_EDGE('',*,*,#5129,.F.);
#6925=ORIENTED_EDGE('',*,*,#5150,.F.);
#6926=ORIENTED_EDGE('',*,*,#5135,.F.);
#6927=ORIENTED_EDGE('',*,*,#5151,.F.);
#6928=ORIENTED_EDGE('',*,*,#5152,.F.);
#6929=ORIENTED_EDGE('',*,*,#5153,.F.);
#6930=ORIENTED_EDGE('',*,*,#5154,.F.);
#6931=ORIENTED_EDGE('',*,*,#5155,.F.);
#6932=ORIENTED_EDGE('',*,*,#5156,.F.);
#6933=ORIENTED_EDGE('',*,*,#5157,.F.);
#6934=ORIENTED_EDGE('',*,*,#5158,.F.);
#6935=ORIENTED_EDGE('',*,*,#5159,.T.);
#6936=ORIENTED_EDGE('',*,*,#5133,.F.);
#6937=ORIENTED_EDGE('',*,*,#5159,.F.);
#6938=ORIENTED_EDGE('',*,*,#5160,.F.);
#6939=ORIENTED_EDGE('',*,*,#5151,.T.);
#6940=ORIENTED_EDGE('',*,*,#5134,.F.);
#6941=ORIENTED_EDGE('',*,*,#5150,.T.);
#6942=ORIENTED_EDGE('',*,*,#5161,.T.);
#6943=ORIENTED_EDGE('',*,*,#5162,.T.);
#6944=ORIENTED_EDGE('',*,*,#5136,.T.);
#6945=ORIENTED_EDGE('',*,*,#5104,.T.);
#6946=ORIENTED_EDGE('',*,*,#5122,.F.);
#6947=ORIENTED_EDGE('',*,*,#5163,.F.);
#6948=ORIENTED_EDGE('',*,*,#5164,.F.);
#6949=ORIENTED_EDGE('',*,*,#5165,.F.);
#6950=ORIENTED_EDGE('',*,*,#5166,.F.);
#6951=ORIENTED_EDGE('',*,*,#5167,.F.);
#6952=ORIENTED_EDGE('',*,*,#5168,.F.);
#6953=ORIENTED_EDGE('',*,*,#5169,.F.);
#6954=ORIENTED_EDGE('',*,*,#5170,.F.);
#6955=ORIENTED_EDGE('',*,*,#5171,.F.);
#6956=ORIENTED_EDGE('',*,*,#5172,.F.);
#6957=ORIENTED_EDGE('',*,*,#5173,.F.);
#6958=ORIENTED_EDGE('',*,*,#5174,.F.);
#6959=ORIENTED_EDGE('',*,*,#5175,.F.);
#6960=ORIENTED_EDGE('',*,*,#5176,.F.);
#6961=ORIENTED_EDGE('',*,*,#5152,.T.);
#6962=ORIENTED_EDGE('',*,*,#5160,.T.);
#6963=ORIENTED_EDGE('',*,*,#5158,.T.);
#6964=ORIENTED_EDGE('',*,*,#5177,.F.);
#6965=ORIENTED_EDGE('',*,*,#5178,.F.);
#6966=ORIENTED_EDGE('',*,*,#5117,.F.);
#6967=ORIENTED_EDGE('',*,*,#5114,.T.);
#6968=ORIENTED_EDGE('',*,*,#5116,.T.);
#6969=ORIENTED_EDGE('',*,*,#5154,.T.);
#6970=ORIENTED_EDGE('',*,*,#5179,.F.);
#6971=ORIENTED_EDGE('',*,*,#5180,.F.);
#6972=ORIENTED_EDGE('',*,*,#5161,.F.);
#6973=ORIENTED_EDGE('',*,*,#5079,.T.);
#6974=ORIENTED_EDGE('',*,*,#5082,.T.);
#6975=ORIENTED_EDGE('',*,*,#5085,.T.);
#6976=ORIENTED_EDGE('',*,*,#5088,.T.);
#6977=ORIENTED_EDGE('',*,*,#5157,.T.);
#6978=ORIENTED_EDGE('',*,*,#5181,.T.);
#6979=ORIENTED_EDGE('',*,*,#5182,.T.);
#6980=ORIENTED_EDGE('',*,*,#5177,.T.);
#6981=ORIENTED_EDGE('',*,*,#5147,.T.);
#6982=ORIENTED_EDGE('',*,*,#5183,.F.);
#6983=ORIENTED_EDGE('',*,*,#5184,.F.);
#6984=ORIENTED_EDGE('',*,*,#5185,.F.);
#6985=ORIENTED_EDGE('',*,*,#5165,.T.);
#6986=ORIENTED_EDGE('',*,*,#5186,.F.);
#6987=ORIENTED_EDGE('',*,*,#5187,.F.);
#6988=ORIENTED_EDGE('',*,*,#5188,.F.);
#6989=ORIENTED_EDGE('',*,*,#5189,.F.);
#6990=ORIENTED_EDGE('',*,*,#5190,.F.);
#6991=ORIENTED_EDGE('',*,*,#5191,.F.);
#6992=ORIENTED_EDGE('',*,*,#5192,.F.);
#6993=ORIENTED_EDGE('',*,*,#5193,.F.);
#6994=ORIENTED_EDGE('',*,*,#5194,.F.);
#6995=ORIENTED_EDGE('',*,*,#5193,.T.);
#6996=ORIENTED_EDGE('',*,*,#5148,.T.);
#6997=ORIENTED_EDGE('',*,*,#5185,.T.);
#6998=ORIENTED_EDGE('',*,*,#5195,.T.);
#6999=ORIENTED_EDGE('',*,*,#5196,.F.);
#7000=ORIENTED_EDGE('',*,*,#5197,.F.);
#7001=ORIENTED_EDGE('',*,*,#5198,.F.);
#7002=ORIENTED_EDGE('',*,*,#5197,.T.);
#7003=ORIENTED_EDGE('',*,*,#5166,.T.);
#7004=ORIENTED_EDGE('',*,*,#5188,.T.);
#7005=ORIENTED_EDGE('',*,*,#5199,.T.);
#7006=ORIENTED_EDGE('',*,*,#5198,.T.);
#7007=ORIENTED_EDGE('',*,*,#5200,.T.);
#7008=ORIENTED_EDGE('',*,*,#5191,.T.);
#7009=ORIENTED_EDGE('',*,*,#5201,.T.);
#7010=ORIENTED_EDGE('',*,*,#5202,.F.);
#7011=ORIENTED_EDGE('',*,*,#5203,.F.);
#7012=ORIENTED_EDGE('',*,*,#5204,.F.);
#7013=ORIENTED_EDGE('',*,*,#5203,.T.);
#7014=ORIENTED_EDGE('',*,*,#5205,.T.);
#7015=ORIENTED_EDGE('',*,*,#5194,.T.);
#7016=ORIENTED_EDGE('',*,*,#5206,.T.);
#7017=ORIENTED_EDGE('',*,*,#5186,.T.);
#7018=ORIENTED_EDGE('',*,*,#5164,.T.);
#7019=ORIENTED_EDGE('',*,*,#5204,.T.);
#7020=ORIENTED_EDGE('',*,*,#5207,.T.);
#7021=ORIENTED_EDGE('',*,*,#5144,.T.);
#7022=ORIENTED_EDGE('',*,*,#5208,.F.);
#7023=ORIENTED_EDGE('',*,*,#5209,.F.);
#7024=ORIENTED_EDGE('',*,*,#5210,.F.);
#7025=ORIENTED_EDGE('',*,*,#5211,.F.);
#7026=ORIENTED_EDGE('',*,*,#5130,.F.);
#7027=ORIENTED_EDGE('',*,*,#5212,.F.);
#7028=ORIENTED_EDGE('',*,*,#5168,.T.);
#7029=ORIENTED_EDGE('',*,*,#5213,.F.);
#7030=ORIENTED_EDGE('',*,*,#5214,.F.);
#7031=ORIENTED_EDGE('',*,*,#5215,.F.);
#7032=ORIENTED_EDGE('',*,*,#5213,.T.);
#7033=ORIENTED_EDGE('',*,*,#5167,.T.);
#7034=ORIENTED_EDGE('',*,*,#5196,.T.);
#7035=ORIENTED_EDGE('',*,*,#5216,.T.);
#7036=ORIENTED_EDGE('',*,*,#5214,.T.);
#7037=ORIENTED_EDGE('',*,*,#5217,.T.);
#7038=ORIENTED_EDGE('',*,*,#5209,.T.);
#7039=ORIENTED_EDGE('',*,*,#5218,.T.);
#7040=ORIENTED_EDGE('',*,*,#5219,.F.);
#7041=ORIENTED_EDGE('',*,*,#5121,.F.);
#7042=ORIENTED_EDGE('',*,*,#5220,.F.);
#7043=ORIENTED_EDGE('',*,*,#5142,.T.);
#7044=ORIENTED_EDGE('',*,*,#5221,.F.);
#7045=ORIENTED_EDGE('',*,*,#5222,.F.);
#7046=ORIENTED_EDGE('',*,*,#5223,.F.);
#7047=ORIENTED_EDGE('',*,*,#5170,.T.);
#7048=ORIENTED_EDGE('',*,*,#5224,.F.);
#7049=ORIENTED_EDGE('',*,*,#5225,.F.);
#7050=ORIENTED_EDGE('',*,*,#5226,.F.);
#7051=ORIENTED_EDGE('',*,*,#5224,.T.);
#7052=ORIENTED_EDGE('',*,*,#5169,.T.);
#7053=ORIENTED_EDGE('',*,*,#5215,.T.);
#7054=ORIENTED_EDGE('',*,*,#5227,.T.);
#7055=ORIENTED_EDGE('',*,*,#5225,.T.);
#7056=ORIENTED_EDGE('',*,*,#5228,.T.);
#7057=ORIENTED_EDGE('',*,*,#5222,.T.);
#7058=ORIENTED_EDGE('',*,*,#5229,.T.);
#7059=ORIENTED_EDGE('',*,*,#5230,.F.);
#7060=ORIENTED_EDGE('',*,*,#5231,.F.);
#7061=ORIENTED_EDGE('',*,*,#5232,.F.);
#7062=ORIENTED_EDGE('',*,*,#5233,.F.);
#7063=ORIENTED_EDGE('',*,*,#5234,.F.);
#7064=ORIENTED_EDGE('',*,*,#5235,.F.);
#7065=ORIENTED_EDGE('',*,*,#5236,.T.);
#7066=ORIENTED_EDGE('',*,*,#5234,.T.);
#7067=ORIENTED_EDGE('',*,*,#5131,.T.);
#7068=ORIENTED_EDGE('',*,*,#5127,.T.);
#7069=ORIENTED_EDGE('',*,*,#5237,.F.);
#7070=ORIENTED_EDGE('',*,*,#5238,.F.);
#7071=ORIENTED_EDGE('',*,*,#5239,.F.);
#7072=ORIENTED_EDGE('',*,*,#5238,.T.);
#7073=ORIENTED_EDGE('',*,*,#5171,.T.);
#7074=ORIENTED_EDGE('',*,*,#5226,.T.);
#7075=ORIENTED_EDGE('',*,*,#5240,.T.);
#7076=ORIENTED_EDGE('',*,*,#5239,.T.);
#7077=ORIENTED_EDGE('',*,*,#5241,.T.);
#7078=ORIENTED_EDGE('',*,*,#5232,.T.);
#7079=ORIENTED_EDGE('',*,*,#5242,.T.);
#7080=ORIENTED_EDGE('',*,*,#5182,.F.);
#7081=ORIENTED_EDGE('',*,*,#5243,.F.);
#7082=ORIENTED_EDGE('',*,*,#5244,.F.);
#7083=ORIENTED_EDGE('',*,*,#5243,.T.);
#7084=ORIENTED_EDGE('',*,*,#5245,.T.);
#7085=ORIENTED_EDGE('',*,*,#5235,.T.);
#7086=ORIENTED_EDGE('',*,*,#5246,.T.);
#7087=ORIENTED_EDGE('',*,*,#5178,.T.);
#7088=ORIENTED_EDGE('',*,*,#5244,.T.);
#7089=ORIENTED_EDGE('',*,*,#5247,.T.);
#7090=ORIENTED_EDGE('',*,*,#5118,.F.);
#7091=ORIENTED_EDGE('',*,*,#5139,.T.);
#7092=ORIENTED_EDGE('',*,*,#5248,.F.);
#7093=ORIENTED_EDGE('',*,*,#5249,.F.);
#7094=ORIENTED_EDGE('',*,*,#5250,.F.);
#7095=ORIENTED_EDGE('',*,*,#5251,.F.);
#7096=ORIENTED_EDGE('',*,*,#5162,.F.);
#7097=ORIENTED_EDGE('',*,*,#5252,.F.);
#7098=ORIENTED_EDGE('',*,*,#5155,.T.);
#7099=ORIENTED_EDGE('',*,*,#5132,.T.);
#7100=ORIENTED_EDGE('',*,*,#5233,.T.);
#7101=ORIENTED_EDGE('',*,*,#5253,.T.);
#7102=ORIENTED_EDGE('',*,*,#5173,.T.);
#7103=ORIENTED_EDGE('',*,*,#5254,.F.);
#7104=ORIENTED_EDGE('',*,*,#5255,.F.);
#7105=ORIENTED_EDGE('',*,*,#5256,.F.);
#7106=ORIENTED_EDGE('',*,*,#5257,.F.);
#7107=ORIENTED_EDGE('',*,*,#5258,.F.);
#7108=ORIENTED_EDGE('',*,*,#5259,.F.);
#7109=ORIENTED_EDGE('',*,*,#5153,.T.);
#7110=ORIENTED_EDGE('',*,*,#5176,.T.);
#7111=ORIENTED_EDGE('',*,*,#5258,.T.);
#7112=ORIENTED_EDGE('',*,*,#5179,.T.);
#7113=ORIENTED_EDGE('',*,*,#5260,.F.);
#7114=ORIENTED_EDGE('',*,*,#5261,.F.);
#7115=ORIENTED_EDGE('',*,*,#5262,.F.);
#7116=ORIENTED_EDGE('',*,*,#5248,.T.);
#7117=ORIENTED_EDGE('',*,*,#5138,.T.);
#7118=ORIENTED_EDGE('',*,*,#5261,.T.);
#7119=ORIENTED_EDGE('',*,*,#5263,.T.);
#7120=ORIENTED_EDGE('',*,*,#5251,.T.);
#7121=ORIENTED_EDGE('',*,*,#5264,.T.);
#7122=ORIENTED_EDGE('',*,*,#5262,.T.);
#7123=ORIENTED_EDGE('',*,*,#5137,.T.);
#7124=ORIENTED_EDGE('',*,*,#5265,.F.);
#7125=ORIENTED_EDGE('',*,*,#5266,.F.);
#7126=ORIENTED_EDGE('',*,*,#5267,.F.);
#7127=ORIENTED_EDGE('',*,*,#5260,.T.);
#7128=ORIENTED_EDGE('',*,*,#5268,.T.);
#7129=ORIENTED_EDGE('',*,*,#5266,.T.);
#7130=ORIENTED_EDGE('',*,*,#5269,.T.);
#7131=ORIENTED_EDGE('',*,*,#5267,.T.);
#7132=ORIENTED_EDGE('',*,*,#5270,.T.);
#7133=ORIENTED_EDGE('',*,*,#5259,.T.);
#7134=ORIENTED_EDGE('',*,*,#5175,.T.);
#7135=ORIENTED_EDGE('',*,*,#5265,.T.);
#7136=ORIENTED_EDGE('',*,*,#5174,.T.);
#7137=ORIENTED_EDGE('',*,*,#5256,.T.);
#7138=ORIENTED_EDGE('',*,*,#5271,.T.);
#7139=ORIENTED_EDGE('',*,*,#5257,.T.);
#7140=ORIENTED_EDGE('',*,*,#5272,.T.);
#7141=ORIENTED_EDGE('',*,*,#5252,.T.);
#7142=ORIENTED_EDGE('',*,*,#5180,.T.);
#7143=ORIENTED_EDGE('',*,*,#5254,.T.);
#7144=ORIENTED_EDGE('',*,*,#5172,.T.);
#7145=ORIENTED_EDGE('',*,*,#5237,.T.);
#7146=ORIENTED_EDGE('',*,*,#5273,.T.);
#7147=ORIENTED_EDGE('',*,*,#5255,.T.);
#7148=ORIENTED_EDGE('',*,*,#5274,.T.);
#7149=ORIENTED_EDGE('',*,*,#5249,.T.);
#7150=ORIENTED_EDGE('',*,*,#5275,.T.);
#7151=ORIENTED_EDGE('',*,*,#5231,.T.);
#7152=ORIENTED_EDGE('',*,*,#5140,.T.);
#7153=ORIENTED_EDGE('',*,*,#5250,.T.);
#7154=ORIENTED_EDGE('',*,*,#5276,.T.);
#7155=ORIENTED_EDGE('',*,*,#5221,.T.);
#7156=ORIENTED_EDGE('',*,*,#5141,.T.);
#7157=ORIENTED_EDGE('',*,*,#5230,.T.);
#7158=ORIENTED_EDGE('',*,*,#5277,.T.);
#7159=ORIENTED_EDGE('',*,*,#5208,.T.);
#7160=ORIENTED_EDGE('',*,*,#5143,.T.);
#7161=ORIENTED_EDGE('',*,*,#5223,.T.);
#7162=ORIENTED_EDGE('',*,*,#5278,.T.);
#7163=ORIENTED_EDGE('',*,*,#5211,.T.);
#7164=ORIENTED_EDGE('',*,*,#5279,.T.);
#7165=ORIENTED_EDGE('',*,*,#5220,.T.);
#7166=ORIENTED_EDGE('',*,*,#5126,.T.);
#7167=ORIENTED_EDGE('',*,*,#5219,.T.);
#7168=ORIENTED_EDGE('',*,*,#5280,.T.);
#7169=ORIENTED_EDGE('',*,*,#5202,.T.);
#7170=ORIENTED_EDGE('',*,*,#5163,.T.);
#7171=ORIENTED_EDGE('',*,*,#5192,.T.);
#7172=ORIENTED_EDGE('',*,*,#5281,.T.);
#7173=ORIENTED_EDGE('',*,*,#5212,.T.);
#7174=ORIENTED_EDGE('',*,*,#5149,.T.);
#7175=ORIENTED_EDGE('',*,*,#5190,.T.);
#7176=ORIENTED_EDGE('',*,*,#5145,.T.);
#7177=ORIENTED_EDGE('',*,*,#5210,.T.);
#7178=ORIENTED_EDGE('',*,*,#5282,.T.);
#7179=ORIENTED_EDGE('',*,*,#5183,.T.);
#7180=ORIENTED_EDGE('',*,*,#5146,.T.);
#7181=ORIENTED_EDGE('',*,*,#5189,.T.);
#7182=ORIENTED_EDGE('',*,*,#5283,.T.);
#7183=ORIENTED_EDGE('',*,*,#5187,.T.);
#7184=ORIENTED_EDGE('',*,*,#5284,.T.);
#7185=ORIENTED_EDGE('',*,*,#5184,.T.);
#7186=ORIENTED_EDGE('',*,*,#5285,.T.);
#7187=ORIENTED_EDGE('',*,*,#5247,.F.);
#7188=ORIENTED_EDGE('',*,*,#5246,.F.);
#7189=ORIENTED_EDGE('',*,*,#5236,.F.);
#7190=ORIENTED_EDGE('',*,*,#5123,.F.);
#7191=ORIENTED_EDGE('',*,*,#5195,.F.);
#7192=ORIENTED_EDGE('',*,*,#5284,.F.);
#7193=ORIENTED_EDGE('',*,*,#5207,.F.);
#7194=ORIENTED_EDGE('',*,*,#5206,.F.);
#7195=ORIENTED_EDGE('',*,*,#5199,.F.);
#7196=ORIENTED_EDGE('',*,*,#5285,.F.);
#7197=ORIENTED_EDGE('',*,*,#5283,.F.);
#7198=ORIENTED_EDGE('',*,*,#5200,.F.);
#7199=ORIENTED_EDGE('',*,*,#5201,.F.);
#7200=ORIENTED_EDGE('',*,*,#5282,.F.);
#7201=ORIENTED_EDGE('',*,*,#5217,.F.);
#7202=ORIENTED_EDGE('',*,*,#5216,.F.);
#7203=ORIENTED_EDGE('',*,*,#5218,.F.);
#7204=ORIENTED_EDGE('',*,*,#5278,.F.);
#7205=ORIENTED_EDGE('',*,*,#5228,.F.);
#7206=ORIENTED_EDGE('',*,*,#5227,.F.);
#7207=ORIENTED_EDGE('',*,*,#5229,.F.);
#7208=ORIENTED_EDGE('',*,*,#5277,.F.);
#7209=ORIENTED_EDGE('',*,*,#5241,.F.);
#7210=ORIENTED_EDGE('',*,*,#5240,.F.);
#7211=ORIENTED_EDGE('',*,*,#5242,.F.);
#7212=ORIENTED_EDGE('',*,*,#5276,.F.);
#7213=ORIENTED_EDGE('',*,*,#5274,.F.);
#7214=ORIENTED_EDGE('',*,*,#5273,.F.);
#7215=ORIENTED_EDGE('',*,*,#5156,.T.);
#7216=ORIENTED_EDGE('',*,*,#5253,.F.);
#7217=ORIENTED_EDGE('',*,*,#5245,.F.);
#7218=ORIENTED_EDGE('',*,*,#5181,.F.);
#7219=ORIENTED_EDGE('',*,*,#5263,.F.);
#7220=ORIENTED_EDGE('',*,*,#5269,.F.);
#7221=ORIENTED_EDGE('',*,*,#5271,.F.);
#7222=ORIENTED_EDGE('',*,*,#5275,.F.);
#7223=ORIENTED_EDGE('',*,*,#5264,.F.);
#7224=ORIENTED_EDGE('',*,*,#5272,.F.);
#7225=ORIENTED_EDGE('',*,*,#5270,.F.);
#7226=ORIENTED_EDGE('',*,*,#5268,.F.);
#7227=ORIENTED_EDGE('',*,*,#5279,.F.);
#7228=ORIENTED_EDGE('',*,*,#5281,.F.);
#7229=ORIENTED_EDGE('',*,*,#5205,.F.);
#7230=ORIENTED_EDGE('',*,*,#5280,.F.);
#7231=ORIENTED_EDGE('',*,*,#5286,.F.);
#7232=ORIENTED_EDGE('',*,*,#5287,.F.);
#7233=ORIENTED_EDGE('',*,*,#5288,.F.);
#7234=ORIENTED_EDGE('',*,*,#5289,.F.);
#7235=ORIENTED_EDGE('',*,*,#5290,.F.);
#7236=ORIENTED_EDGE('',*,*,#5291,.F.);
#7237=ORIENTED_EDGE('',*,*,#5288,.T.);
#7238=ORIENTED_EDGE('',*,*,#5292,.F.);
#7239=ORIENTED_EDGE('',*,*,#5293,.F.);
#7240=ORIENTED_EDGE('',*,*,#5294,.F.);
#7241=ORIENTED_EDGE('',*,*,#5290,.T.);
#7242=ORIENTED_EDGE('',*,*,#5295,.F.);
#7243=ORIENTED_EDGE('',*,*,#5286,.T.);
#7244=ORIENTED_EDGE('',*,*,#5296,.F.);
#7245=ORIENTED_EDGE('',*,*,#5293,.T.);
#7246=ORIENTED_EDGE('',*,*,#5297,.F.);
#7247=ORIENTED_EDGE('',*,*,#5291,.T.);
#7248=ORIENTED_EDGE('',*,*,#5298,.F.);
#7249=ORIENTED_EDGE('',*,*,#5299,.T.);
#7250=ORIENTED_EDGE('',*,*,#5300,.T.);
#7251=ORIENTED_EDGE('',*,*,#5289,.T.);
#7252=ORIENTED_EDGE('',*,*,#5300,.F.);
#7253=ORIENTED_EDGE('',*,*,#5301,.T.);
#7254=ORIENTED_EDGE('',*,*,#5302,.T.);
#7255=ORIENTED_EDGE('',*,*,#5303,.T.);
#7256=ORIENTED_EDGE('',*,*,#5304,.T.);
#7257=ORIENTED_EDGE('',*,*,#5305,.T.);
#7258=ORIENTED_EDGE('',*,*,#5306,.T.);
#7259=ORIENTED_EDGE('',*,*,#5287,.T.);
#7260=ORIENTED_EDGE('',*,*,#5297,.T.);
#7261=ORIENTED_EDGE('',*,*,#5295,.T.);
#7262=ORIENTED_EDGE('',*,*,#5292,.T.);
#7263=ORIENTED_EDGE('',*,*,#5307,.T.);
#7264=ORIENTED_EDGE('',*,*,#5308,.F.);
#7265=ORIENTED_EDGE('',*,*,#5309,.T.);
#7266=ORIENTED_EDGE('',*,*,#5310,.T.);
#7267=ORIENTED_EDGE('',*,*,#5311,.T.);
#7268=ORIENTED_EDGE('',*,*,#5312,.T.);
#7269=ORIENTED_EDGE('',*,*,#5313,.T.);
#7270=ORIENTED_EDGE('',*,*,#5314,.F.);
#7271=ORIENTED_EDGE('',*,*,#5315,.T.);
#7272=ORIENTED_EDGE('',*,*,#5316,.T.);
#7273=ORIENTED_EDGE('',*,*,#5317,.T.);
#7274=ORIENTED_EDGE('',*,*,#5318,.F.);
#7275=ORIENTED_EDGE('',*,*,#5319,.F.);
#7276=ORIENTED_EDGE('',*,*,#5320,.F.);
#7277=ORIENTED_EDGE('',*,*,#5317,.F.);
#7278=ORIENTED_EDGE('',*,*,#5321,.T.);
#7279=ORIENTED_EDGE('',*,*,#5322,.T.);
#7280=ORIENTED_EDGE('',*,*,#5323,.T.);
#7281=ORIENTED_EDGE('',*,*,#5324,.T.);
#7282=ORIENTED_EDGE('',*,*,#5325,.T.);
#7283=ORIENTED_EDGE('',*,*,#5326,.T.);
#7284=ORIENTED_EDGE('',*,*,#5327,.F.);
#7285=ORIENTED_EDGE('',*,*,#5319,.T.);
#7286=ORIENTED_EDGE('',*,*,#5328,.F.);
#7287=ORIENTED_EDGE('',*,*,#5326,.F.);
#7288=ORIENTED_EDGE('',*,*,#5329,.T.);
#7289=ORIENTED_EDGE('',*,*,#5330,.T.);
#7290=ORIENTED_EDGE('',*,*,#5331,.T.);
#7291=ORIENTED_EDGE('',*,*,#5332,.T.);
#7292=ORIENTED_EDGE('',*,*,#5333,.T.);
#7293=ORIENTED_EDGE('',*,*,#5334,.T.);
#7294=ORIENTED_EDGE('',*,*,#5335,.T.);
#7295=ORIENTED_EDGE('',*,*,#5336,.T.);
#7296=ORIENTED_EDGE('',*,*,#5337,.T.);
#7297=ORIENTED_EDGE('',*,*,#5338,.T.);
#7298=ORIENTED_EDGE('',*,*,#5339,.T.);
#7299=ORIENTED_EDGE('',*,*,#5340,.T.);
#7300=ORIENTED_EDGE('',*,*,#5340,.F.);
#7301=ORIENTED_EDGE('',*,*,#5341,.F.);
#7302=ORIENTED_EDGE('',*,*,#5325,.F.);
#7303=ORIENTED_EDGE('',*,*,#5342,.F.);
#7304=ORIENTED_EDGE('',*,*,#5343,.T.);
#7305=ORIENTED_EDGE('',*,*,#5344,.T.);
#7306=ORIENTED_EDGE('',*,*,#5345,.T.);
#7307=ORIENTED_EDGE('',*,*,#5339,.F.);
#7308=ORIENTED_EDGE('',*,*,#5346,.F.);
#7309=ORIENTED_EDGE('',*,*,#5345,.F.);
#7310=ORIENTED_EDGE('',*,*,#5347,.F.);
#7311=ORIENTED_EDGE('',*,*,#5344,.F.);
#7312=ORIENTED_EDGE('',*,*,#5348,.F.);
#7313=ORIENTED_EDGE('',*,*,#5334,.F.);
#7314=ORIENTED_EDGE('',*,*,#5349,.F.);
#7315=ORIENTED_EDGE('',*,*,#5337,.F.);
#7316=ORIENTED_EDGE('',*,*,#5350,.F.);
#7317=ORIENTED_EDGE('',*,*,#5343,.F.);
#7318=ORIENTED_EDGE('',*,*,#5351,.F.);
#7319=ORIENTED_EDGE('',*,*,#5331,.F.);
#7320=ORIENTED_EDGE('',*,*,#5352,.F.);
#7321=ORIENTED_EDGE('',*,*,#5338,.F.);
#7322=ORIENTED_EDGE('',*,*,#5353,.F.);
#7323=ORIENTED_EDGE('',*,*,#5321,.F.);
#7324=ORIENTED_EDGE('',*,*,#5354,.F.);
#7325=ORIENTED_EDGE('',*,*,#5336,.F.);
#7326=ORIENTED_EDGE('',*,*,#5355,.F.);
#7327=ORIENTED_EDGE('',*,*,#5335,.F.);
#7328=ORIENTED_EDGE('',*,*,#5356,.F.);
#7329=ORIENTED_EDGE('',*,*,#5330,.F.);
#7330=ORIENTED_EDGE('',*,*,#5357,.F.);
#7331=ORIENTED_EDGE('',*,*,#5333,.F.);
#7332=ORIENTED_EDGE('',*,*,#5303,.F.);
#7333=ORIENTED_EDGE('',*,*,#5315,.F.);
#7334=ORIENTED_EDGE('',*,*,#5358,.F.);
#7335=ORIENTED_EDGE('',*,*,#5323,.F.);
#7336=ORIENTED_EDGE('',*,*,#5304,.F.);
#7337=ORIENTED_EDGE('',*,*,#5332,.F.);
#7338=ORIENTED_EDGE('',*,*,#5359,.F.);
#7339=ORIENTED_EDGE('',*,*,#5329,.F.);
#7340=ORIENTED_EDGE('',*,*,#5360,.F.);
#7341=ORIENTED_EDGE('',*,*,#5312,.F.);
#7342=ORIENTED_EDGE('',*,*,#5361,.F.);
#7343=ORIENTED_EDGE('',*,*,#5313,.F.);
#7344=ORIENTED_EDGE('',*,*,#5362,.F.);
#7345=ORIENTED_EDGE('',*,*,#5324,.F.);
#7346=ORIENTED_EDGE('',*,*,#5363,.F.);
#7347=ORIENTED_EDGE('',*,*,#5307,.F.);
#7348=ORIENTED_EDGE('',*,*,#5305,.F.);
#7349=ORIENTED_EDGE('',*,*,#5322,.F.);
#7350=ORIENTED_EDGE('',*,*,#5364,.F.);
#7351=ORIENTED_EDGE('',*,*,#5310,.F.);
#7352=ORIENTED_EDGE('',*,*,#5365,.F.);
#7353=ORIENTED_EDGE('',*,*,#5316,.F.);
#7354=ORIENTED_EDGE('',*,*,#5306,.F.);
#7355=ORIENTED_EDGE('',*,*,#5366,.F.);
#7356=ORIENTED_EDGE('',*,*,#5367,.F.);
#7357=ORIENTED_EDGE('',*,*,#5368,.F.);
#7358=ORIENTED_EDGE('',*,*,#5311,.F.);
#7359=ORIENTED_EDGE('',*,*,#5369,.F.);
#7360=ORIENTED_EDGE('',*,*,#5367,.T.);
#7361=ORIENTED_EDGE('',*,*,#5370,.F.);
#7362=ORIENTED_EDGE('',*,*,#5309,.F.);
#7363=ORIENTED_EDGE('',*,*,#5370,.T.);
#7364=ORIENTED_EDGE('',*,*,#5371,.F.);
#7365=ORIENTED_EDGE('',*,*,#5318,.T.);
#7366=ORIENTED_EDGE('',*,*,#5365,.T.);
#7367=ORIENTED_EDGE('',*,*,#5314,.T.);
#7368=ORIENTED_EDGE('',*,*,#5320,.T.);
#7369=ORIENTED_EDGE('',*,*,#5327,.T.);
#7370=ORIENTED_EDGE('',*,*,#5341,.T.);
#7371=ORIENTED_EDGE('',*,*,#5347,.T.);
#7372=ORIENTED_EDGE('',*,*,#5349,.T.);
#7373=ORIENTED_EDGE('',*,*,#5358,.T.);
#7374=ORIENTED_EDGE('',*,*,#5342,.T.);
#7375=ORIENTED_EDGE('',*,*,#5362,.T.);
#7376=ORIENTED_EDGE('',*,*,#5360,.T.);
#7377=ORIENTED_EDGE('',*,*,#5353,.T.);
#7378=ORIENTED_EDGE('',*,*,#5346,.T.);
#7379=ORIENTED_EDGE('',*,*,#5352,.T.);
#7380=ORIENTED_EDGE('',*,*,#5356,.T.);
#7381=ORIENTED_EDGE('',*,*,#5351,.T.);
#7382=ORIENTED_EDGE('',*,*,#5372,.T.);
#7383=ORIENTED_EDGE('',*,*,#5373,.T.);
#7384=ORIENTED_EDGE('',*,*,#5374,.T.);
#7385=ORIENTED_EDGE('',*,*,#5375,.T.);
#7386=ORIENTED_EDGE('',*,*,#5348,.T.);
#7387=ORIENTED_EDGE('',*,*,#5350,.T.);
#7388=ORIENTED_EDGE('',*,*,#5354,.T.);
#7389=ORIENTED_EDGE('',*,*,#5359,.T.);
#7390=ORIENTED_EDGE('',*,*,#5355,.T.);
#7391=ORIENTED_EDGE('',*,*,#5357,.T.);
#7392=ORIENTED_EDGE('',*,*,#5361,.T.);
#7393=ORIENTED_EDGE('',*,*,#5368,.T.);
#7394=ORIENTED_EDGE('',*,*,#5369,.T.);
#7395=ORIENTED_EDGE('',*,*,#5308,.T.);
#7396=ORIENTED_EDGE('',*,*,#5364,.T.);
#7397=ORIENTED_EDGE('',*,*,#5376,.F.);
#7398=ORIENTED_EDGE('',*,*,#5372,.F.);
#7399=ORIENTED_EDGE('',*,*,#5377,.F.);
#7400=ORIENTED_EDGE('',*,*,#5301,.F.);
#7401=ORIENTED_EDGE('',*,*,#5378,.F.);
#7402=ORIENTED_EDGE('',*,*,#5379,.F.);
#7403=ORIENTED_EDGE('',*,*,#5377,.T.);
#7404=ORIENTED_EDGE('',*,*,#5375,.F.);
#7405=ORIENTED_EDGE('',*,*,#5380,.F.);
#7406=ORIENTED_EDGE('',*,*,#5381,.F.);
#7407=ORIENTED_EDGE('',*,*,#5378,.T.);
#7408=ORIENTED_EDGE('',*,*,#5374,.F.);
#7409=ORIENTED_EDGE('',*,*,#5376,.T.);
#7410=ORIENTED_EDGE('',*,*,#5299,.F.);
#7411=ORIENTED_EDGE('',*,*,#5380,.T.);
#7412=ORIENTED_EDGE('',*,*,#5373,.F.);
#7413=ORIENTED_EDGE('',*,*,#5296,.T.);
#7414=ORIENTED_EDGE('',*,*,#5302,.F.);
#7415=ORIENTED_EDGE('',*,*,#5379,.T.);
#7416=ORIENTED_EDGE('',*,*,#5382,.T.);
#7417=ORIENTED_EDGE('',*,*,#5294,.T.);
#7418=ORIENTED_EDGE('',*,*,#5382,.F.);
#7419=ORIENTED_EDGE('',*,*,#5381,.T.);
#7420=ORIENTED_EDGE('',*,*,#5298,.T.);
#7421=ORIENTED_EDGE('',*,*,#5366,.T.);
#7422=ORIENTED_EDGE('',*,*,#5363,.T.);
#7423=ORIENTED_EDGE('',*,*,#5328,.T.);
#7424=ORIENTED_EDGE('',*,*,#5371,.T.);
#7425=ORIENTED_EDGE('',*,*,#5383,.F.);
#7426=ORIENTED_EDGE('',*,*,#5384,.T.);
#7427=ORIENTED_EDGE('',*,*,#5385,.F.);
#7428=ORIENTED_EDGE('',*,*,#5384,.F.);
#7429=ORIENTED_EDGE('',*,*,#5386,.F.);
#7430=ORIENTED_EDGE('',*,*,#5387,.T.);
#7431=ORIENTED_EDGE('',*,*,#5388,.F.);
#7432=ORIENTED_EDGE('',*,*,#5389,.F.);
#7433=ORIENTED_EDGE('',*,*,#5390,.F.);
#7434=ORIENTED_EDGE('',*,*,#5391,.F.);
#7435=ORIENTED_EDGE('',*,*,#5392,.F.);
#7436=ORIENTED_EDGE('',*,*,#5393,.F.);
#7437=ORIENTED_EDGE('',*,*,#5394,.F.);
#7438=ORIENTED_EDGE('',*,*,#5395,.F.);
#7439=ORIENTED_EDGE('',*,*,#5396,.F.);
#7440=ORIENTED_EDGE('',*,*,#5387,.F.);
#7441=ORIENTED_EDGE('',*,*,#5392,.T.);
#7442=ORIENTED_EDGE('',*,*,#5397,.F.);
#7443=ORIENTED_EDGE('',*,*,#5398,.F.);
#7444=ORIENTED_EDGE('',*,*,#5399,.F.);
#7445=ORIENTED_EDGE('',*,*,#5400,.T.);
#7446=ORIENTED_EDGE('',*,*,#5401,.F.);
#7447=ORIENTED_EDGE('',*,*,#5402,.T.);
#7448=ORIENTED_EDGE('',*,*,#5403,.F.);
#7449=ORIENTED_EDGE('',*,*,#5404,.T.);
#7450=ORIENTED_EDGE('',*,*,#5405,.F.);
#7451=ORIENTED_EDGE('',*,*,#5406,.T.);
#7452=ORIENTED_EDGE('',*,*,#5407,.F.);
#7453=ORIENTED_EDGE('',*,*,#5408,.F.);
#7454=ORIENTED_EDGE('',*,*,#5409,.F.);
#7455=ORIENTED_EDGE('',*,*,#5410,.T.);
#7456=ORIENTED_EDGE('',*,*,#5411,.F.);
#7457=ORIENTED_EDGE('',*,*,#5412,.T.);
#7458=ORIENTED_EDGE('',*,*,#5413,.T.);
#7459=ORIENTED_EDGE('',*,*,#5414,.F.);
#7460=ORIENTED_EDGE('',*,*,#5415,.T.);
#7461=ORIENTED_EDGE('',*,*,#5416,.T.);
#7462=ORIENTED_EDGE('',*,*,#5417,.F.);
#7463=ORIENTED_EDGE('',*,*,#5418,.T.);
#7464=ORIENTED_EDGE('',*,*,#5419,.T.);
#7465=ORIENTED_EDGE('',*,*,#5420,.F.);
#7466=ORIENTED_EDGE('',*,*,#5391,.T.);
#7467=ORIENTED_EDGE('',*,*,#5421,.T.);
#7468=ORIENTED_EDGE('',*,*,#5422,.T.);
#7469=ORIENTED_EDGE('',*,*,#5397,.T.);
#7470=ORIENTED_EDGE('',*,*,#5390,.T.);
#7471=ORIENTED_EDGE('',*,*,#5423,.F.);
#7472=ORIENTED_EDGE('',*,*,#5424,.F.);
#7473=ORIENTED_EDGE('',*,*,#5421,.F.);
#7474=ORIENTED_EDGE('',*,*,#5389,.T.);
#7475=ORIENTED_EDGE('',*,*,#5425,.T.);
#7476=ORIENTED_EDGE('',*,*,#5426,.T.);
#7477=ORIENTED_EDGE('',*,*,#5423,.T.);
#7478=ORIENTED_EDGE('',*,*,#5427,.F.);
#7479=ORIENTED_EDGE('',*,*,#5428,.T.);
#7480=ORIENTED_EDGE('',*,*,#5412,.F.);
#7481=ORIENTED_EDGE('',*,*,#5429,.F.);
#7482=ORIENTED_EDGE('',*,*,#5430,.F.);
#7483=ORIENTED_EDGE('',*,*,#5431,.F.);
#7484=ORIENTED_EDGE('',*,*,#5432,.F.);
#7485=ORIENTED_EDGE('',*,*,#5433,.F.);
#7486=ORIENTED_EDGE('',*,*,#5434,.F.);
#7487=ORIENTED_EDGE('',*,*,#5435,.F.);
#7488=ORIENTED_EDGE('',*,*,#5413,.F.);
#7489=ORIENTED_EDGE('',*,*,#5428,.F.);
#7490=ORIENTED_EDGE('',*,*,#5436,.F.);
#7491=ORIENTED_EDGE('',*,*,#5437,.T.);
#7492=ORIENTED_EDGE('',*,*,#5438,.F.);
#7493=ORIENTED_EDGE('',*,*,#5437,.F.);
#7494=ORIENTED_EDGE('',*,*,#5439,.F.);
#7495=ORIENTED_EDGE('',*,*,#5440,.T.);
#7496=ORIENTED_EDGE('',*,*,#5441,.F.);
#7497=ORIENTED_EDGE('',*,*,#5440,.F.);
#7498=ORIENTED_EDGE('',*,*,#5442,.F.);
#7499=ORIENTED_EDGE('',*,*,#5443,.T.);
#7500=ORIENTED_EDGE('',*,*,#5444,.F.);
#7501=ORIENTED_EDGE('',*,*,#5445,.F.);
#7502=ORIENTED_EDGE('',*,*,#5446,.F.);
#7503=ORIENTED_EDGE('',*,*,#5447,.F.);
#7504=ORIENTED_EDGE('',*,*,#5406,.F.);
#7505=ORIENTED_EDGE('',*,*,#5448,.F.);
#7506=ORIENTED_EDGE('',*,*,#5449,.F.);
#7507=ORIENTED_EDGE('',*,*,#5450,.F.);
#7508=ORIENTED_EDGE('',*,*,#5451,.F.);
#7509=ORIENTED_EDGE('',*,*,#5443,.F.);
#7510=ORIENTED_EDGE('',*,*,#5452,.F.);
#7511=ORIENTED_EDGE('',*,*,#5453,.T.);
#7512=ORIENTED_EDGE('',*,*,#5454,.F.);
#7513=ORIENTED_EDGE('',*,*,#5453,.F.);
#7514=ORIENTED_EDGE('',*,*,#5455,.F.);
#7515=ORIENTED_EDGE('',*,*,#5456,.T.);
#7516=ORIENTED_EDGE('',*,*,#5457,.F.);
#7517=ORIENTED_EDGE('',*,*,#5458,.F.);
#7518=ORIENTED_EDGE('',*,*,#5459,.F.);
#7519=ORIENTED_EDGE('',*,*,#5460,.F.);
#7520=ORIENTED_EDGE('',*,*,#5404,.F.);
#7521=ORIENTED_EDGE('',*,*,#5461,.F.);
#7522=ORIENTED_EDGE('',*,*,#5462,.F.);
#7523=ORIENTED_EDGE('',*,*,#5463,.F.);
#7524=ORIENTED_EDGE('',*,*,#5464,.F.);
#7525=ORIENTED_EDGE('',*,*,#5456,.F.);
#7526=ORIENTED_EDGE('',*,*,#5465,.F.);
#7527=ORIENTED_EDGE('',*,*,#5466,.T.);
#7528=ORIENTED_EDGE('',*,*,#5467,.F.);
#7529=ORIENTED_EDGE('',*,*,#5466,.F.);
#7530=ORIENTED_EDGE('',*,*,#5468,.F.);
#7531=ORIENTED_EDGE('',*,*,#5469,.T.);
#7532=ORIENTED_EDGE('',*,*,#5470,.F.);
#7533=ORIENTED_EDGE('',*,*,#5471,.F.);
#7534=ORIENTED_EDGE('',*,*,#5472,.F.);
#7535=ORIENTED_EDGE('',*,*,#5473,.F.);
#7536=ORIENTED_EDGE('',*,*,#5400,.F.);
#7537=ORIENTED_EDGE('',*,*,#5474,.F.);
#7538=ORIENTED_EDGE('',*,*,#5475,.F.);
#7539=ORIENTED_EDGE('',*,*,#5476,.F.);
#7540=ORIENTED_EDGE('',*,*,#5477,.F.);
#7541=ORIENTED_EDGE('',*,*,#5469,.F.);
#7542=ORIENTED_EDGE('',*,*,#5478,.F.);
#7543=ORIENTED_EDGE('',*,*,#5479,.T.);
#7544=ORIENTED_EDGE('',*,*,#5480,.F.);
#7545=ORIENTED_EDGE('',*,*,#5479,.F.);
#7546=ORIENTED_EDGE('',*,*,#5481,.F.);
#7547=ORIENTED_EDGE('',*,*,#5482,.T.);
#7548=ORIENTED_EDGE('',*,*,#5415,.F.);
#7549=ORIENTED_EDGE('',*,*,#5483,.F.);
#7550=ORIENTED_EDGE('',*,*,#5484,.F.);
#7551=ORIENTED_EDGE('',*,*,#5485,.F.);
#7552=ORIENTED_EDGE('',*,*,#5486,.F.);
#7553=ORIENTED_EDGE('',*,*,#5487,.F.);
#7554=ORIENTED_EDGE('',*,*,#5488,.F.);
#7555=ORIENTED_EDGE('',*,*,#5489,.F.);
#7556=ORIENTED_EDGE('',*,*,#5416,.F.);
#7557=ORIENTED_EDGE('',*,*,#5482,.F.);
#7558=ORIENTED_EDGE('',*,*,#5490,.F.);
#7559=ORIENTED_EDGE('',*,*,#5491,.T.);
#7560=ORIENTED_EDGE('',*,*,#5492,.F.);
#7561=ORIENTED_EDGE('',*,*,#5491,.F.);
#7562=ORIENTED_EDGE('',*,*,#5493,.F.);
#7563=ORIENTED_EDGE('',*,*,#5494,.T.);
#7564=ORIENTED_EDGE('',*,*,#5495,.F.);
#7565=ORIENTED_EDGE('',*,*,#5496,.F.);
#7566=ORIENTED_EDGE('',*,*,#5497,.F.);
#7567=ORIENTED_EDGE('',*,*,#5498,.F.);
#7568=ORIENTED_EDGE('',*,*,#5402,.F.);
#7569=ORIENTED_EDGE('',*,*,#5499,.F.);
#7570=ORIENTED_EDGE('',*,*,#5500,.F.);
#7571=ORIENTED_EDGE('',*,*,#5501,.F.);
#7572=ORIENTED_EDGE('',*,*,#5502,.F.);
#7573=ORIENTED_EDGE('',*,*,#5494,.F.);
#7574=ORIENTED_EDGE('',*,*,#5503,.F.);
#7575=ORIENTED_EDGE('',*,*,#5504,.T.);
#7576=ORIENTED_EDGE('',*,*,#5505,.F.);
#7577=ORIENTED_EDGE('',*,*,#5506,.F.);
#7578=ORIENTED_EDGE('',*,*,#5507,.F.);
#7579=ORIENTED_EDGE('',*,*,#5508,.F.);
#7580=ORIENTED_EDGE('',*,*,#5509,.F.);
#7581=ORIENTED_EDGE('',*,*,#5510,.F.);
#7582=ORIENTED_EDGE('',*,*,#5511,.F.);
#7583=ORIENTED_EDGE('',*,*,#5512,.F.);
#7584=ORIENTED_EDGE('',*,*,#5513,.F.);
#7585=ORIENTED_EDGE('',*,*,#5514,.F.);
#7586=ORIENTED_EDGE('',*,*,#5515,.F.);
#7587=ORIENTED_EDGE('',*,*,#5516,.F.);
#7588=ORIENTED_EDGE('',*,*,#5517,.F.);
#7589=ORIENTED_EDGE('',*,*,#5518,.F.);
#7590=ORIENTED_EDGE('',*,*,#5519,.F.);
#7591=ORIENTED_EDGE('',*,*,#5520,.F.);
#7592=ORIENTED_EDGE('',*,*,#5521,.F.);
#7593=ORIENTED_EDGE('',*,*,#5504,.F.);
#7594=ORIENTED_EDGE('',*,*,#5522,.F.);
#7595=ORIENTED_EDGE('',*,*,#5523,.T.);
#7596=ORIENTED_EDGE('',*,*,#5524,.F.);
#7597=ORIENTED_EDGE('',*,*,#5525,.F.);
#7598=ORIENTED_EDGE('',*,*,#5526,.F.);
#7599=ORIENTED_EDGE('',*,*,#5527,.F.);
#7600=ORIENTED_EDGE('',*,*,#5410,.F.);
#7601=ORIENTED_EDGE('',*,*,#5528,.F.);
#7602=ORIENTED_EDGE('',*,*,#5529,.F.);
#7603=ORIENTED_EDGE('',*,*,#5530,.F.);
#7604=ORIENTED_EDGE('',*,*,#5531,.F.);
#7605=ORIENTED_EDGE('',*,*,#5523,.F.);
#7606=ORIENTED_EDGE('',*,*,#5532,.F.);
#7607=ORIENTED_EDGE('',*,*,#5533,.T.);
#7608=ORIENTED_EDGE('',*,*,#5534,.F.);
#7609=ORIENTED_EDGE('',*,*,#5535,.F.);
#7610=ORIENTED_EDGE('',*,*,#5536,.F.);
#7611=ORIENTED_EDGE('',*,*,#5537,.F.);
#7612=ORIENTED_EDGE('',*,*,#5538,.F.);
#7613=ORIENTED_EDGE('',*,*,#5539,.F.);
#7614=ORIENTED_EDGE('',*,*,#5540,.F.);
#7615=ORIENTED_EDGE('',*,*,#5541,.F.);
#7616=ORIENTED_EDGE('',*,*,#5542,.F.);
#7617=ORIENTED_EDGE('',*,*,#5543,.F.);
#7618=ORIENTED_EDGE('',*,*,#5544,.F.);
#7619=ORIENTED_EDGE('',*,*,#5545,.F.);
#7620=ORIENTED_EDGE('',*,*,#5546,.F.);
#7621=ORIENTED_EDGE('',*,*,#5547,.F.);
#7622=ORIENTED_EDGE('',*,*,#5548,.F.);
#7623=ORIENTED_EDGE('',*,*,#5549,.F.);
#7624=ORIENTED_EDGE('',*,*,#5550,.F.);
#7625=ORIENTED_EDGE('',*,*,#5533,.F.);
#7626=ORIENTED_EDGE('',*,*,#5551,.F.);
#7627=ORIENTED_EDGE('',*,*,#5552,.T.);
#7628=ORIENTED_EDGE('',*,*,#5553,.F.);
#7629=ORIENTED_EDGE('',*,*,#5554,.F.);
#7630=ORIENTED_EDGE('',*,*,#5555,.F.);
#7631=ORIENTED_EDGE('',*,*,#5556,.F.);
#7632=ORIENTED_EDGE('',*,*,#5557,.F.);
#7633=ORIENTED_EDGE('',*,*,#5558,.F.);
#7634=ORIENTED_EDGE('',*,*,#5559,.F.);
#7635=ORIENTED_EDGE('',*,*,#5560,.F.);
#7636=ORIENTED_EDGE('',*,*,#5561,.F.);
#7637=ORIENTED_EDGE('',*,*,#5562,.F.);
#7638=ORIENTED_EDGE('',*,*,#5563,.F.);
#7639=ORIENTED_EDGE('',*,*,#5564,.F.);
#7640=ORIENTED_EDGE('',*,*,#5565,.F.);
#7641=ORIENTED_EDGE('',*,*,#5566,.F.);
#7642=ORIENTED_EDGE('',*,*,#5567,.F.);
#7643=ORIENTED_EDGE('',*,*,#5568,.F.);
#7644=ORIENTED_EDGE('',*,*,#5569,.F.);
#7645=ORIENTED_EDGE('',*,*,#5552,.F.);
#7646=ORIENTED_EDGE('',*,*,#5570,.F.);
#7647=ORIENTED_EDGE('',*,*,#5571,.T.);
#7648=ORIENTED_EDGE('',*,*,#5572,.F.);
#7649=ORIENTED_EDGE('',*,*,#5573,.F.);
#7650=ORIENTED_EDGE('',*,*,#5574,.F.);
#7651=ORIENTED_EDGE('',*,*,#5575,.F.);
#7652=ORIENTED_EDGE('',*,*,#5576,.F.);
#7653=ORIENTED_EDGE('',*,*,#5577,.F.);
#7654=ORIENTED_EDGE('',*,*,#5578,.F.);
#7655=ORIENTED_EDGE('',*,*,#5579,.F.);
#7656=ORIENTED_EDGE('',*,*,#5580,.F.);
#7657=ORIENTED_EDGE('',*,*,#5581,.F.);
#7658=ORIENTED_EDGE('',*,*,#5582,.F.);
#7659=ORIENTED_EDGE('',*,*,#5583,.F.);
#7660=ORIENTED_EDGE('',*,*,#5584,.F.);
#7661=ORIENTED_EDGE('',*,*,#5585,.F.);
#7662=ORIENTED_EDGE('',*,*,#5586,.F.);
#7663=ORIENTED_EDGE('',*,*,#5587,.F.);
#7664=ORIENTED_EDGE('',*,*,#5588,.F.);
#7665=ORIENTED_EDGE('',*,*,#5571,.F.);
#7666=ORIENTED_EDGE('',*,*,#5589,.F.);
#7667=ORIENTED_EDGE('',*,*,#5590,.T.);
#7668=ORIENTED_EDGE('',*,*,#5591,.F.);
#7669=ORIENTED_EDGE('',*,*,#5590,.F.);
#7670=ORIENTED_EDGE('',*,*,#5592,.F.);
#7671=ORIENTED_EDGE('',*,*,#5593,.T.);
#7672=ORIENTED_EDGE('',*,*,#5418,.F.);
#7673=ORIENTED_EDGE('',*,*,#5594,.F.);
#7674=ORIENTED_EDGE('',*,*,#5595,.F.);
#7675=ORIENTED_EDGE('',*,*,#5596,.F.);
#7676=ORIENTED_EDGE('',*,*,#5597,.F.);
#7677=ORIENTED_EDGE('',*,*,#5598,.F.);
#7678=ORIENTED_EDGE('',*,*,#5599,.F.);
#7679=ORIENTED_EDGE('',*,*,#5600,.F.);
#7680=ORIENTED_EDGE('',*,*,#5419,.F.);
#7681=ORIENTED_EDGE('',*,*,#5593,.F.);
#7682=ORIENTED_EDGE('',*,*,#5473,.T.);
#7683=ORIENTED_EDGE('',*,*,#5601,.T.);
#7684=ORIENTED_EDGE('',*,*,#5499,.T.);
#7685=ORIENTED_EDGE('',*,*,#5401,.T.);
#7686=ORIENTED_EDGE('',*,*,#5474,.T.);
#7687=ORIENTED_EDGE('',*,*,#5399,.T.);
#7688=ORIENTED_EDGE('',*,*,#5602,.T.);
#7689=ORIENTED_EDGE('',*,*,#5603,.T.);
#7690=ORIENTED_EDGE('',*,*,#5461,.T.);
#7691=ORIENTED_EDGE('',*,*,#5403,.T.);
#7692=ORIENTED_EDGE('',*,*,#5498,.T.);
#7693=ORIENTED_EDGE('',*,*,#5604,.T.);
#7694=ORIENTED_EDGE('',*,*,#5447,.T.);
#7695=ORIENTED_EDGE('',*,*,#5605,.T.);
#7696=ORIENTED_EDGE('',*,*,#5606,.T.);
#7697=ORIENTED_EDGE('',*,*,#5407,.T.);
#7698=ORIENTED_EDGE('',*,*,#5448,.T.);
#7699=ORIENTED_EDGE('',*,*,#5405,.T.);
#7700=ORIENTED_EDGE('',*,*,#5460,.T.);
#7701=ORIENTED_EDGE('',*,*,#5607,.T.);
#7702=ORIENTED_EDGE('',*,*,#5446,.T.);
#7703=ORIENTED_EDGE('',*,*,#5608,.F.);
#7704=ORIENTED_EDGE('',*,*,#5609,.F.);
#7705=ORIENTED_EDGE('',*,*,#5605,.F.);
#7706=ORIENTED_EDGE('',*,*,#5472,.T.);
#7707=ORIENTED_EDGE('',*,*,#5610,.F.);
#7708=ORIENTED_EDGE('',*,*,#5500,.T.);
#7709=ORIENTED_EDGE('',*,*,#5601,.F.);
#7710=ORIENTED_EDGE('',*,*,#5475,.T.);
#7711=ORIENTED_EDGE('',*,*,#5603,.F.);
#7712=ORIENTED_EDGE('',*,*,#5611,.F.);
#7713=ORIENTED_EDGE('',*,*,#5612,.F.);
#7714=ORIENTED_EDGE('',*,*,#5462,.T.);
#7715=ORIENTED_EDGE('',*,*,#5604,.F.);
#7716=ORIENTED_EDGE('',*,*,#5497,.T.);
#7717=ORIENTED_EDGE('',*,*,#5613,.F.);
#7718=ORIENTED_EDGE('',*,*,#5471,.T.);
#7719=ORIENTED_EDGE('',*,*,#5614,.T.);
#7720=ORIENTED_EDGE('',*,*,#5501,.T.);
#7721=ORIENTED_EDGE('',*,*,#5610,.T.);
#7722=ORIENTED_EDGE('',*,*,#5476,.T.);
#7723=ORIENTED_EDGE('',*,*,#5612,.T.);
#7724=ORIENTED_EDGE('',*,*,#5615,.T.);
#7725=ORIENTED_EDGE('',*,*,#5616,.T.);
#7726=ORIENTED_EDGE('',*,*,#5463,.T.);
#7727=ORIENTED_EDGE('',*,*,#5613,.T.);
#7728=ORIENTED_EDGE('',*,*,#5496,.T.);
#7729=ORIENTED_EDGE('',*,*,#5617,.T.);
#7730=ORIENTED_EDGE('',*,*,#5445,.T.);
#7731=ORIENTED_EDGE('',*,*,#5618,.T.);
#7732=ORIENTED_EDGE('',*,*,#5619,.T.);
#7733=ORIENTED_EDGE('',*,*,#5608,.T.);
#7734=ORIENTED_EDGE('',*,*,#5577,.T.);
#7735=ORIENTED_EDGE('',*,*,#5620,.T.);
#7736=ORIENTED_EDGE('',*,*,#5621,.T.);
#7737=ORIENTED_EDGE('',*,*,#5622,.T.);
#7738=ORIENTED_EDGE('',*,*,#5558,.T.);
#7739=ORIENTED_EDGE('',*,*,#5623,.T.);
#7740=ORIENTED_EDGE('',*,*,#5575,.T.);
#7741=ORIENTED_EDGE('',*,*,#5624,.T.);
#7742=ORIENTED_EDGE('',*,*,#5537,.T.);
#7743=ORIENTED_EDGE('',*,*,#5625,.T.);
#7744=ORIENTED_EDGE('',*,*,#5626,.T.);
#7745=ORIENTED_EDGE('',*,*,#5627,.T.);
#7746=ORIENTED_EDGE('',*,*,#5508,.T.);
#7747=ORIENTED_EDGE('',*,*,#5628,.T.);
#7748=ORIENTED_EDGE('',*,*,#5539,.T.);
#7749=ORIENTED_EDGE('',*,*,#5629,.T.);
#7750=ORIENTED_EDGE('',*,*,#5510,.T.);
#7751=ORIENTED_EDGE('',*,*,#5630,.T.);
#7752=ORIENTED_EDGE('',*,*,#5556,.T.);
#7753=ORIENTED_EDGE('',*,*,#5631,.T.);
#7754=ORIENTED_EDGE('',*,*,#5578,.T.);
#7755=ORIENTED_EDGE('',*,*,#5622,.F.);
#7756=ORIENTED_EDGE('',*,*,#5632,.F.);
#7757=ORIENTED_EDGE('',*,*,#5633,.F.);
#7758=ORIENTED_EDGE('',*,*,#5559,.T.);
#7759=ORIENTED_EDGE('',*,*,#5624,.F.);
#7760=ORIENTED_EDGE('',*,*,#5574,.T.);
#7761=ORIENTED_EDGE('',*,*,#5634,.F.);
#7762=ORIENTED_EDGE('',*,*,#5536,.T.);
#7763=ORIENTED_EDGE('',*,*,#5635,.F.);
#7764=ORIENTED_EDGE('',*,*,#5636,.F.);
#7765=ORIENTED_EDGE('',*,*,#5625,.F.);
#7766=ORIENTED_EDGE('',*,*,#5507,.T.);
#7767=ORIENTED_EDGE('',*,*,#5637,.F.);
#7768=ORIENTED_EDGE('',*,*,#5540,.T.);
#7769=ORIENTED_EDGE('',*,*,#5628,.F.);
#7770=ORIENTED_EDGE('',*,*,#5511,.T.);
#7771=ORIENTED_EDGE('',*,*,#5631,.F.);
#7772=ORIENTED_EDGE('',*,*,#5555,.T.);
#7773=ORIENTED_EDGE('',*,*,#5638,.F.);
#7774=ORIENTED_EDGE('',*,*,#5583,.T.);
#7775=ORIENTED_EDGE('',*,*,#5639,.T.);
#7776=ORIENTED_EDGE('',*,*,#5640,.T.);
#7777=ORIENTED_EDGE('',*,*,#5641,.T.);
#7778=ORIENTED_EDGE('',*,*,#5564,.T.);
#7779=ORIENTED_EDGE('',*,*,#5642,.T.);
#7780=ORIENTED_EDGE('',*,*,#5585,.T.);
#7781=ORIENTED_EDGE('',*,*,#5643,.T.);
#7782=ORIENTED_EDGE('',*,*,#5547,.T.);
#7783=ORIENTED_EDGE('',*,*,#5644,.T.);
#7784=ORIENTED_EDGE('',*,*,#5645,.T.);
#7785=ORIENTED_EDGE('',*,*,#5646,.T.);
#7786=ORIENTED_EDGE('',*,*,#5518,.T.);
#7787=ORIENTED_EDGE('',*,*,#5647,.T.);
#7788=ORIENTED_EDGE('',*,*,#5545,.T.);
#7789=ORIENTED_EDGE('',*,*,#5648,.T.);
#7790=ORIENTED_EDGE('',*,*,#5579,.T.);
#7791=ORIENTED_EDGE('',*,*,#5633,.T.);
#7792=ORIENTED_EDGE('',*,*,#5649,.T.);
#7793=ORIENTED_EDGE('',*,*,#5650,.T.);
#7794=ORIENTED_EDGE('',*,*,#5560,.T.);
#7795=ORIENTED_EDGE('',*,*,#5634,.T.);
#7796=ORIENTED_EDGE('',*,*,#5573,.T.);
#7797=ORIENTED_EDGE('',*,*,#5651,.T.);
#7798=ORIENTED_EDGE('',*,*,#5535,.T.);
#7799=ORIENTED_EDGE('',*,*,#5652,.T.);
#7800=ORIENTED_EDGE('',*,*,#5653,.T.);
#7801=ORIENTED_EDGE('',*,*,#5635,.T.);
#7802=ORIENTED_EDGE('',*,*,#5506,.T.);
#7803=ORIENTED_EDGE('',*,*,#5654,.T.);
#7804=ORIENTED_EDGE('',*,*,#5541,.T.);
#7805=ORIENTED_EDGE('',*,*,#5637,.T.);
#7806=ORIENTED_EDGE('',*,*,#5512,.T.);
#7807=ORIENTED_EDGE('',*,*,#5638,.T.);
#7808=ORIENTED_EDGE('',*,*,#5554,.T.);
#7809=ORIENTED_EDGE('',*,*,#5655,.T.);
#7810=ORIENTED_EDGE('',*,*,#5582,.T.);
#7811=ORIENTED_EDGE('',*,*,#5656,.F.);
#7812=ORIENTED_EDGE('',*,*,#5657,.F.);
#7813=ORIENTED_EDGE('',*,*,#5639,.F.);
#7814=ORIENTED_EDGE('',*,*,#5563,.T.);
#7815=ORIENTED_EDGE('',*,*,#5658,.F.);
#7816=ORIENTED_EDGE('',*,*,#5586,.T.);
#7817=ORIENTED_EDGE('',*,*,#5642,.F.);
#7818=ORIENTED_EDGE('',*,*,#5548,.T.);
#7819=ORIENTED_EDGE('',*,*,#5646,.F.);
#7820=ORIENTED_EDGE('',*,*,#5659,.F.);
#7821=ORIENTED_EDGE('',*,*,#5660,.F.);
#7822=ORIENTED_EDGE('',*,*,#5519,.T.);
#7823=ORIENTED_EDGE('',*,*,#5648,.F.);
#7824=ORIENTED_EDGE('',*,*,#5544,.T.);
#7825=ORIENTED_EDGE('',*,*,#5661,.F.);
#7826=ORIENTED_EDGE('',*,*,#5534,.T.);
#7827=ORIENTED_EDGE('',*,*,#5550,.T.);
#7828=ORIENTED_EDGE('',*,*,#5662,.F.);
#7829=ORIENTED_EDGE('',*,*,#5663,.F.);
#7830=ORIENTED_EDGE('',*,*,#5652,.F.);
#7831=ORIENTED_EDGE('',*,*,#5580,.T.);
#7832=ORIENTED_EDGE('',*,*,#5650,.F.);
#7833=ORIENTED_EDGE('',*,*,#5664,.F.);
#7834=ORIENTED_EDGE('',*,*,#5665,.F.);
#7835=ORIENTED_EDGE('',*,*,#5561,.T.);
#7836=ORIENTED_EDGE('',*,*,#5651,.F.);
#7837=ORIENTED_EDGE('',*,*,#5572,.T.);
#7838=ORIENTED_EDGE('',*,*,#5588,.T.);
#7839=ORIENTED_EDGE('',*,*,#5666,.F.);
#7840=ORIENTED_EDGE('',*,*,#5505,.T.);
#7841=ORIENTED_EDGE('',*,*,#5521,.T.);
#7842=ORIENTED_EDGE('',*,*,#5667,.F.);
#7843=ORIENTED_EDGE('',*,*,#5542,.T.);
#7844=ORIENTED_EDGE('',*,*,#5654,.F.);
#7845=ORIENTED_EDGE('',*,*,#5581,.T.);
#7846=ORIENTED_EDGE('',*,*,#5665,.T.);
#7847=ORIENTED_EDGE('',*,*,#5668,.T.);
#7848=ORIENTED_EDGE('',*,*,#5656,.T.);
#7849=ORIENTED_EDGE('',*,*,#5562,.T.);
#7850=ORIENTED_EDGE('',*,*,#5666,.T.);
#7851=ORIENTED_EDGE('',*,*,#5587,.T.);
#7852=ORIENTED_EDGE('',*,*,#5658,.T.);
#7853=ORIENTED_EDGE('',*,*,#5549,.T.);
#7854=ORIENTED_EDGE('',*,*,#5660,.T.);
#7855=ORIENTED_EDGE('',*,*,#5669,.T.);
#7856=ORIENTED_EDGE('',*,*,#5662,.T.);
#7857=ORIENTED_EDGE('',*,*,#5520,.T.);
#7858=ORIENTED_EDGE('',*,*,#5661,.T.);
#7859=ORIENTED_EDGE('',*,*,#5543,.T.);
#7860=ORIENTED_EDGE('',*,*,#5667,.T.);
#7861=ORIENTED_EDGE('',*,*,#5388,.T.);
#7862=ORIENTED_EDGE('',*,*,#5396,.T.);
#7863=ORIENTED_EDGE('',*,*,#5670,.F.);
#7864=ORIENTED_EDGE('',*,*,#5597,.T.);
#7865=ORIENTED_EDGE('',*,*,#5671,.F.);
#7866=ORIENTED_EDGE('',*,*,#5486,.T.);
#7867=ORIENTED_EDGE('',*,*,#5672,.F.);
#7868=ORIENTED_EDGE('',*,*,#5432,.T.);
#7869=ORIENTED_EDGE('',*,*,#5673,.F.);
#7870=ORIENTED_EDGE('',*,*,#5524,.T.);
#7871=ORIENTED_EDGE('',*,*,#5531,.T.);
#7872=ORIENTED_EDGE('',*,*,#5674,.F.);
#7873=ORIENTED_EDGE('',*,*,#5675,.F.);
#7874=ORIENTED_EDGE('',*,*,#5676,.F.);
#7875=ORIENTED_EDGE('',*,*,#5677,.F.);
#7876=ORIENTED_EDGE('',*,*,#5425,.F.);
#7877=ORIENTED_EDGE('',*,*,#5395,.T.);
#7878=ORIENTED_EDGE('',*,*,#5678,.T.);
#7879=ORIENTED_EDGE('',*,*,#5598,.T.);
#7880=ORIENTED_EDGE('',*,*,#5670,.T.);
#7881=ORIENTED_EDGE('',*,*,#5530,.T.);
#7882=ORIENTED_EDGE('',*,*,#5679,.T.);
#7883=ORIENTED_EDGE('',*,*,#5680,.T.);
#7884=ORIENTED_EDGE('',*,*,#5674,.T.);
#7885=ORIENTED_EDGE('',*,*,#5487,.T.);
#7886=ORIENTED_EDGE('',*,*,#5671,.T.);
#7887=ORIENTED_EDGE('',*,*,#5596,.T.);
#7888=ORIENTED_EDGE('',*,*,#5681,.T.);
#7889=ORIENTED_EDGE('',*,*,#5431,.T.);
#7890=ORIENTED_EDGE('',*,*,#5682,.T.);
#7891=ORIENTED_EDGE('',*,*,#5525,.T.);
#7892=ORIENTED_EDGE('',*,*,#5673,.T.);
#7893=ORIENTED_EDGE('',*,*,#5433,.T.);
#7894=ORIENTED_EDGE('',*,*,#5672,.T.);
#7895=ORIENTED_EDGE('',*,*,#5485,.T.);
#7896=ORIENTED_EDGE('',*,*,#5683,.T.);
#7897=ORIENTED_EDGE('',*,*,#5529,.T.);
#7898=ORIENTED_EDGE('',*,*,#5684,.F.);
#7899=ORIENTED_EDGE('',*,*,#5685,.F.);
#7900=ORIENTED_EDGE('',*,*,#5679,.F.);
#7901=ORIENTED_EDGE('',*,*,#5394,.T.);
#7902=ORIENTED_EDGE('',*,*,#5686,.F.);
#7903=ORIENTED_EDGE('',*,*,#5599,.T.);
#7904=ORIENTED_EDGE('',*,*,#5678,.F.);
#7905=ORIENTED_EDGE('',*,*,#5430,.T.);
#7906=ORIENTED_EDGE('',*,*,#5687,.F.);
#7907=ORIENTED_EDGE('',*,*,#5526,.T.);
#7908=ORIENTED_EDGE('',*,*,#5682,.F.);
#7909=ORIENTED_EDGE('',*,*,#5488,.T.);
#7910=ORIENTED_EDGE('',*,*,#5681,.F.);
#7911=ORIENTED_EDGE('',*,*,#5595,.T.);
#7912=ORIENTED_EDGE('',*,*,#5688,.F.);
#7913=ORIENTED_EDGE('',*,*,#5393,.T.);
#7914=ORIENTED_EDGE('',*,*,#5420,.T.);
#7915=ORIENTED_EDGE('',*,*,#5600,.T.);
#7916=ORIENTED_EDGE('',*,*,#5686,.T.);
#7917=ORIENTED_EDGE('',*,*,#5528,.T.);
#7918=ORIENTED_EDGE('',*,*,#5409,.T.);
#7919=ORIENTED_EDGE('',*,*,#5689,.T.);
#7920=ORIENTED_EDGE('',*,*,#5684,.T.);
#7921=ORIENTED_EDGE('',*,*,#5489,.T.);
#7922=ORIENTED_EDGE('',*,*,#5688,.T.);
#7923=ORIENTED_EDGE('',*,*,#5594,.T.);
#7924=ORIENTED_EDGE('',*,*,#5417,.T.);
#7925=ORIENTED_EDGE('',*,*,#5429,.T.);
#7926=ORIENTED_EDGE('',*,*,#5411,.T.);
#7927=ORIENTED_EDGE('',*,*,#5527,.T.);
#7928=ORIENTED_EDGE('',*,*,#5687,.T.);
#7929=ORIENTED_EDGE('',*,*,#5444,.T.);
#7930=ORIENTED_EDGE('',*,*,#5451,.T.);
#7931=ORIENTED_EDGE('',*,*,#5690,.F.);
#7932=ORIENTED_EDGE('',*,*,#5457,.T.);
#7933=ORIENTED_EDGE('',*,*,#5464,.T.);
#7934=ORIENTED_EDGE('',*,*,#5617,.F.);
#7935=ORIENTED_EDGE('',*,*,#5495,.T.);
#7936=ORIENTED_EDGE('',*,*,#5502,.T.);
#7937=ORIENTED_EDGE('',*,*,#5614,.F.);
#7938=ORIENTED_EDGE('',*,*,#5470,.T.);
#7939=ORIENTED_EDGE('',*,*,#5477,.T.);
#7940=ORIENTED_EDGE('',*,*,#5616,.F.);
#7941=ORIENTED_EDGE('',*,*,#5691,.F.);
#7942=ORIENTED_EDGE('',*,*,#5620,.F.);
#7943=ORIENTED_EDGE('',*,*,#5576,.T.);
#7944=ORIENTED_EDGE('',*,*,#5623,.F.);
#7945=ORIENTED_EDGE('',*,*,#5557,.T.);
#7946=ORIENTED_EDGE('',*,*,#5630,.F.);
#7947=ORIENTED_EDGE('',*,*,#5509,.T.);
#7948=ORIENTED_EDGE('',*,*,#5629,.F.);
#7949=ORIENTED_EDGE('',*,*,#5538,.T.);
#7950=ORIENTED_EDGE('',*,*,#5627,.F.);
#7951=ORIENTED_EDGE('',*,*,#5692,.F.);
#7952=ORIENTED_EDGE('',*,*,#5618,.F.);
#7953=ORIENTED_EDGE('',*,*,#5467,.T.);
#7954=ORIENTED_EDGE('',*,*,#5441,.T.);
#7955=ORIENTED_EDGE('',*,*,#5438,.T.);
#7956=ORIENTED_EDGE('',*,*,#5517,.T.);
#7957=ORIENTED_EDGE('',*,*,#5693,.F.);
#7958=ORIENTED_EDGE('',*,*,#5565,.T.);
#7959=ORIENTED_EDGE('',*,*,#5643,.F.);
#7960=ORIENTED_EDGE('',*,*,#5584,.T.);
#7961=ORIENTED_EDGE('',*,*,#5641,.F.);
#7962=ORIENTED_EDGE('',*,*,#5694,.F.);
#7963=ORIENTED_EDGE('',*,*,#5695,.F.);
#7964=ORIENTED_EDGE('',*,*,#5696,.F.);
#7965=ORIENTED_EDGE('',*,*,#5644,.F.);
#7966=ORIENTED_EDGE('',*,*,#5546,.T.);
#7967=ORIENTED_EDGE('',*,*,#5647,.F.);
#7968=ORIENTED_EDGE('',*,*,#5385,.T.);
#7969=ORIENTED_EDGE('',*,*,#5591,.T.);
#7970=ORIENTED_EDGE('',*,*,#5492,.T.);
#7971=ORIENTED_EDGE('',*,*,#5480,.T.);
#7972=ORIENTED_EDGE('',*,*,#5454,.T.);
#7973=ORIENTED_EDGE('',*,*,#5669,.F.);
#7974=ORIENTED_EDGE('',*,*,#5697,.F.);
#7975=ORIENTED_EDGE('',*,*,#5698,.F.);
#7976=ORIENTED_EDGE('',*,*,#5699,.F.);
#7977=ORIENTED_EDGE('',*,*,#5700,.F.);
#7978=ORIENTED_EDGE('',*,*,#5668,.F.);
#7979=ORIENTED_EDGE('',*,*,#5653,.F.);
#7980=ORIENTED_EDGE('',*,*,#5701,.F.);
#7981=ORIENTED_EDGE('',*,*,#5702,.T.);
#7982=ORIENTED_EDGE('',*,*,#5703,.F.);
#7983=ORIENTED_EDGE('',*,*,#5701,.T.);
#7984=ORIENTED_EDGE('',*,*,#5663,.T.);
#7985=ORIENTED_EDGE('',*,*,#5698,.T.);
#7986=ORIENTED_EDGE('',*,*,#5704,.T.);
#7987=ORIENTED_EDGE('',*,*,#5705,.T.);
#7988=ORIENTED_EDGE('',*,*,#5706,.F.);
#7989=ORIENTED_EDGE('',*,*,#5645,.F.);
#7990=ORIENTED_EDGE('',*,*,#5707,.F.);
#7991=ORIENTED_EDGE('',*,*,#5649,.F.);
#7992=ORIENTED_EDGE('',*,*,#5708,.F.);
#7993=ORIENTED_EDGE('',*,*,#5709,.T.);
#7994=ORIENTED_EDGE('',*,*,#5710,.F.);
#7995=ORIENTED_EDGE('',*,*,#5711,.T.);
#7996=ORIENTED_EDGE('',*,*,#5712,.F.);
#7997=ORIENTED_EDGE('',*,*,#5640,.F.);
#7998=ORIENTED_EDGE('',*,*,#5713,.F.);
#7999=ORIENTED_EDGE('',*,*,#5713,.T.);
#8000=ORIENTED_EDGE('',*,*,#5657,.T.);
#8001=ORIENTED_EDGE('',*,*,#5700,.T.);
#8002=ORIENTED_EDGE('',*,*,#5714,.T.);
#8003=ORIENTED_EDGE('',*,*,#5626,.F.);
#8004=ORIENTED_EDGE('',*,*,#5715,.F.);
#8005=ORIENTED_EDGE('',*,*,#5716,.F.);
#8006=ORIENTED_EDGE('',*,*,#5715,.T.);
#8007=ORIENTED_EDGE('',*,*,#5636,.T.);
#8008=ORIENTED_EDGE('',*,*,#5703,.T.);
#8009=ORIENTED_EDGE('',*,*,#5717,.T.);
#8010=ORIENTED_EDGE('',*,*,#5718,.F.);
#8011=ORIENTED_EDGE('',*,*,#5719,.F.);
#8012=ORIENTED_EDGE('',*,*,#5720,.F.);
#8013=ORIENTED_EDGE('',*,*,#5719,.T.);
#8014=ORIENTED_EDGE('',*,*,#5721,.T.);
#8015=ORIENTED_EDGE('',*,*,#5707,.T.);
#8016=ORIENTED_EDGE('',*,*,#5696,.T.);
#8017=ORIENTED_EDGE('',*,*,#5621,.F.);
#8018=ORIENTED_EDGE('',*,*,#5722,.F.);
#8019=ORIENTED_EDGE('',*,*,#5723,.F.);
#8020=ORIENTED_EDGE('',*,*,#5724,.F.);
#8021=ORIENTED_EDGE('',*,*,#5725,.F.);
#8022=ORIENTED_EDGE('',*,*,#5726,.F.);
#8023=ORIENTED_EDGE('',*,*,#5712,.T.);
#8024=ORIENTED_EDGE('',*,*,#5727,.T.);
#8025=ORIENTED_EDGE('',*,*,#5725,.T.);
#8026=ORIENTED_EDGE('',*,*,#5694,.T.);
#8027=ORIENTED_EDGE('',*,*,#5619,.F.);
#8028=ORIENTED_EDGE('',*,*,#5728,.F.);
#8029=ORIENTED_EDGE('',*,*,#5729,.F.);
#8030=ORIENTED_EDGE('',*,*,#5728,.T.);
#8031=ORIENTED_EDGE('',*,*,#5692,.T.);
#8032=ORIENTED_EDGE('',*,*,#5716,.T.);
#8033=ORIENTED_EDGE('',*,*,#5730,.T.);
#8034=ORIENTED_EDGE('',*,*,#5731,.F.);
#8035=ORIENTED_EDGE('',*,*,#5732,.F.);
#8036=ORIENTED_EDGE('',*,*,#5733,.F.);
#8037=ORIENTED_EDGE('',*,*,#5732,.T.);
#8038=ORIENTED_EDGE('',*,*,#5734,.T.);
#8039=ORIENTED_EDGE('',*,*,#5718,.T.);
#8040=ORIENTED_EDGE('',*,*,#5735,.T.);
#8041=ORIENTED_EDGE('',*,*,#5615,.F.);
#8042=ORIENTED_EDGE('',*,*,#5736,.F.);
#8043=ORIENTED_EDGE('',*,*,#5737,.F.);
#8044=ORIENTED_EDGE('',*,*,#5738,.F.);
#8045=ORIENTED_EDGE('',*,*,#5739,.F.);
#8046=ORIENTED_EDGE('',*,*,#5740,.F.);
#8047=ORIENTED_EDGE('',*,*,#5739,.T.);
#8048=ORIENTED_EDGE('',*,*,#5741,.T.);
#8049=ORIENTED_EDGE('',*,*,#5726,.T.);
#8050=ORIENTED_EDGE('',*,*,#5742,.T.);
#8051=ORIENTED_EDGE('',*,*,#5606,.F.);
#8052=ORIENTED_EDGE('',*,*,#5743,.F.);
#8053=ORIENTED_EDGE('',*,*,#5744,.T.);
#8054=ORIENTED_EDGE('',*,*,#5745,.F.);
#8055=ORIENTED_EDGE('',*,*,#5743,.T.);
#8056=ORIENTED_EDGE('',*,*,#5609,.T.);
#8057=ORIENTED_EDGE('',*,*,#5729,.T.);
#8058=ORIENTED_EDGE('',*,*,#5746,.T.);
#8059=ORIENTED_EDGE('',*,*,#5747,.F.);
#8060=ORIENTED_EDGE('',*,*,#5748,.F.);
#8061=ORIENTED_EDGE('',*,*,#5749,.F.);
#8062=ORIENTED_EDGE('',*,*,#5602,.F.);
#8063=ORIENTED_EDGE('',*,*,#5750,.F.);
#8064=ORIENTED_EDGE('',*,*,#5751,.T.);
#8065=ORIENTED_EDGE('',*,*,#5752,.F.);
#8066=ORIENTED_EDGE('',*,*,#5753,.F.);
#8067=ORIENTED_EDGE('',*,*,#5754,.F.);
#8068=ORIENTED_EDGE('',*,*,#5755,.F.);
#8069=ORIENTED_EDGE('',*,*,#5689,.F.);
#8070=ORIENTED_EDGE('',*,*,#5756,.F.);
#8071=ORIENTED_EDGE('',*,*,#5757,.F.);
#8072=ORIENTED_EDGE('',*,*,#5756,.T.);
#8073=ORIENTED_EDGE('',*,*,#5408,.T.);
#8074=ORIENTED_EDGE('',*,*,#5745,.T.);
#8075=ORIENTED_EDGE('',*,*,#5758,.T.);
#8076=ORIENTED_EDGE('',*,*,#5759,.F.);
#8077=ORIENTED_EDGE('',*,*,#5760,.F.);
#8078=ORIENTED_EDGE('',*,*,#5761,.F.);
#8079=ORIENTED_EDGE('',*,*,#5422,.F.);
#8080=ORIENTED_EDGE('',*,*,#5762,.F.);
#8081=ORIENTED_EDGE('',*,*,#5763,.F.);
#8082=ORIENTED_EDGE('',*,*,#5764,.F.);
#8083=ORIENTED_EDGE('',*,*,#5765,.F.);
#8084=ORIENTED_EDGE('',*,*,#5766,.F.);
#8085=ORIENTED_EDGE('',*,*,#5680,.F.);
#8086=ORIENTED_EDGE('',*,*,#5767,.F.);
#8087=ORIENTED_EDGE('',*,*,#5768,.T.);
#8088=ORIENTED_EDGE('',*,*,#5769,.F.);
#8089=ORIENTED_EDGE('',*,*,#5767,.T.);
#8090=ORIENTED_EDGE('',*,*,#5685,.T.);
#8091=ORIENTED_EDGE('',*,*,#5757,.T.);
#8092=ORIENTED_EDGE('',*,*,#5770,.T.);
#8093=ORIENTED_EDGE('',*,*,#5769,.T.);
#8094=ORIENTED_EDGE('',*,*,#5771,.T.);
#8095=ORIENTED_EDGE('',*,*,#5761,.T.);
#8096=ORIENTED_EDGE('',*,*,#5675,.T.);
#8097=ORIENTED_EDGE('',*,*,#5426,.F.);
#8098=ORIENTED_EDGE('',*,*,#5772,.F.);
#8099=ORIENTED_EDGE('',*,*,#5773,.T.);
#8100=ORIENTED_EDGE('',*,*,#5774,.F.);
#8101=ORIENTED_EDGE('',*,*,#5765,.T.);
#8102=ORIENTED_EDGE('',*,*,#5775,.T.);
#8103=ORIENTED_EDGE('',*,*,#5772,.T.);
#8104=ORIENTED_EDGE('',*,*,#5677,.T.);
#8105=ORIENTED_EDGE('',*,*,#5762,.T.);
#8106=ORIENTED_EDGE('',*,*,#5424,.T.);
#8107=ORIENTED_EDGE('',*,*,#5774,.T.);
#8108=ORIENTED_EDGE('',*,*,#5776,.T.);
#8109=ORIENTED_EDGE('',*,*,#5760,.T.);
#8110=ORIENTED_EDGE('',*,*,#5777,.T.);
#8111=ORIENTED_EDGE('',*,*,#5766,.T.);
#8112=ORIENTED_EDGE('',*,*,#5676,.T.);
#8113=ORIENTED_EDGE('',*,*,#5754,.T.);
#8114=ORIENTED_EDGE('',*,*,#5778,.T.);
#8115=ORIENTED_EDGE('',*,*,#5764,.T.);
#8116=ORIENTED_EDGE('',*,*,#5779,.T.);
#8117=ORIENTED_EDGE('',*,*,#5750,.T.);
#8118=ORIENTED_EDGE('',*,*,#5398,.T.);
#8119=ORIENTED_EDGE('',*,*,#5763,.T.);
#8120=ORIENTED_EDGE('',*,*,#5780,.T.);
#8121=ORIENTED_EDGE('',*,*,#5435,.T.);
#8122=ORIENTED_EDGE('',*,*,#5781,.T.);
#8123=ORIENTED_EDGE('',*,*,#5483,.T.);
#8124=ORIENTED_EDGE('',*,*,#5414,.T.);
#8125=ORIENTED_EDGE('',*,*,#5748,.T.);
#8126=ORIENTED_EDGE('',*,*,#5782,.T.);
#8127=ORIENTED_EDGE('',*,*,#5759,.T.);
#8128=ORIENTED_EDGE('',*,*,#5783,.T.);
#8129=ORIENTED_EDGE('',*,*,#5747,.T.);
#8130=ORIENTED_EDGE('',*,*,#5784,.T.);
#8131=ORIENTED_EDGE('',*,*,#5755,.T.);
#8132=ORIENTED_EDGE('',*,*,#5785,.T.);
#8133=ORIENTED_EDGE('',*,*,#5753,.T.);
#8134=ORIENTED_EDGE('',*,*,#5786,.T.);
#8135=ORIENTED_EDGE('',*,*,#5740,.T.);
#8136=ORIENTED_EDGE('',*,*,#5787,.T.);
#8137=ORIENTED_EDGE('',*,*,#5736,.T.);
#8138=ORIENTED_EDGE('',*,*,#5611,.T.);
#8139=ORIENTED_EDGE('',*,*,#5752,.T.);
#8140=ORIENTED_EDGE('',*,*,#5788,.T.);
#8141=ORIENTED_EDGE('',*,*,#5731,.T.);
#8142=ORIENTED_EDGE('',*,*,#5789,.T.);
#8143=ORIENTED_EDGE('',*,*,#5749,.T.);
#8144=ORIENTED_EDGE('',*,*,#5790,.T.);
#8145=ORIENTED_EDGE('',*,*,#5738,.T.);
#8146=ORIENTED_EDGE('',*,*,#5791,.T.);
#8147=ORIENTED_EDGE('',*,*,#5733,.T.);
#8148=ORIENTED_EDGE('',*,*,#5792,.T.);
#8149=ORIENTED_EDGE('',*,*,#5722,.T.);
#8150=ORIENTED_EDGE('',*,*,#5691,.T.);
#8151=ORIENTED_EDGE('',*,*,#5737,.T.);
#8152=ORIENTED_EDGE('',*,*,#5793,.T.);
#8153=ORIENTED_EDGE('',*,*,#5450,.T.);
#8154=ORIENTED_EDGE('',*,*,#5794,.T.);
#8155=ORIENTED_EDGE('',*,*,#5458,.T.);
#8156=ORIENTED_EDGE('',*,*,#5690,.T.);
#8157=ORIENTED_EDGE('',*,*,#5724,.T.);
#8158=ORIENTED_EDGE('',*,*,#5795,.T.);
#8159=ORIENTED_EDGE('',*,*,#5720,.T.);
#8160=ORIENTED_EDGE('',*,*,#5695,.T.);
#8161=ORIENTED_EDGE('',*,*,#5708,.T.);
#8162=ORIENTED_EDGE('',*,*,#5632,.T.);
#8163=ORIENTED_EDGE('',*,*,#5723,.T.);
#8164=ORIENTED_EDGE('',*,*,#5796,.T.);
#8165=ORIENTED_EDGE('',*,*,#5516,.T.);
#8166=ORIENTED_EDGE('',*,*,#5797,.T.);
#8167=ORIENTED_EDGE('',*,*,#5566,.T.);
#8168=ORIENTED_EDGE('',*,*,#5693,.T.);
#8169=ORIENTED_EDGE('',*,*,#5699,.T.);
#8170=ORIENTED_EDGE('',*,*,#5664,.T.);
#8171=ORIENTED_EDGE('',*,*,#5710,.T.);
#8172=ORIENTED_EDGE('',*,*,#5798,.T.);
#8173=ORIENTED_EDGE('',*,*,#5697,.T.);
#8174=ORIENTED_EDGE('',*,*,#5659,.T.);
#8175=ORIENTED_EDGE('',*,*,#5706,.T.);
#8176=ORIENTED_EDGE('',*,*,#5799,.T.);
#8177=ORIENTED_EDGE('',*,*,#5514,.T.);
#8178=ORIENTED_EDGE('',*,*,#5800,.T.);
#8179=ORIENTED_EDGE('',*,*,#5568,.T.);
#8180=ORIENTED_EDGE('',*,*,#5801,.T.);
#8181=ORIENTED_EDGE('',*,*,#5711,.F.);
#8182=ORIENTED_EDGE('',*,*,#5714,.F.);
#8183=ORIENTED_EDGE('',*,*,#5798,.F.);
#8184=ORIENTED_EDGE('',*,*,#5709,.F.);
#8185=ORIENTED_EDGE('',*,*,#5796,.F.);
#8186=ORIENTED_EDGE('',*,*,#5793,.F.);
#8187=ORIENTED_EDGE('',*,*,#5788,.F.);
#8188=ORIENTED_EDGE('',*,*,#5751,.F.);
#8189=ORIENTED_EDGE('',*,*,#5780,.F.);
#8190=ORIENTED_EDGE('',*,*,#5776,.F.);
#8191=ORIENTED_EDGE('',*,*,#5773,.F.);
#8192=ORIENTED_EDGE('',*,*,#5775,.F.);
#8193=ORIENTED_EDGE('',*,*,#5778,.F.);
#8194=ORIENTED_EDGE('',*,*,#5787,.F.);
#8195=ORIENTED_EDGE('',*,*,#5742,.F.);
#8196=ORIENTED_EDGE('',*,*,#5727,.F.);
#8197=ORIENTED_EDGE('',*,*,#5515,.T.);
#8198=ORIENTED_EDGE('',*,*,#5801,.F.);
#8199=ORIENTED_EDGE('',*,*,#5567,.T.);
#8200=ORIENTED_EDGE('',*,*,#5797,.F.);
#8201=ORIENTED_EDGE('',*,*,#5741,.F.);
#8202=ORIENTED_EDGE('',*,*,#5792,.F.);
#8203=ORIENTED_EDGE('',*,*,#5735,.F.);
#8204=ORIENTED_EDGE('',*,*,#5795,.F.);
#8205=ORIENTED_EDGE('',*,*,#5434,.T.);
#8206=ORIENTED_EDGE('',*,*,#5683,.F.);
#8207=ORIENTED_EDGE('',*,*,#5484,.T.);
#8208=ORIENTED_EDGE('',*,*,#5781,.F.);
#8209=ORIENTED_EDGE('',*,*,#5777,.F.);
#8210=ORIENTED_EDGE('',*,*,#5782,.F.);
#8211=ORIENTED_EDGE('',*,*,#5785,.F.);
#8212=ORIENTED_EDGE('',*,*,#5779,.F.);
#8213=ORIENTED_EDGE('',*,*,#5784,.F.);
#8214=ORIENTED_EDGE('',*,*,#5789,.F.);
#8215=ORIENTED_EDGE('',*,*,#5791,.F.);
#8216=ORIENTED_EDGE('',*,*,#5786,.F.);
#8217=ORIENTED_EDGE('',*,*,#5427,.T.);
#8218=ORIENTED_EDGE('',*,*,#5436,.T.);
#8219=ORIENTED_EDGE('',*,*,#5439,.T.);
#8220=ORIENTED_EDGE('',*,*,#5442,.T.);
#8221=ORIENTED_EDGE('',*,*,#5452,.T.);
#8222=ORIENTED_EDGE('',*,*,#5455,.T.);
#8223=ORIENTED_EDGE('',*,*,#5465,.T.);
#8224=ORIENTED_EDGE('',*,*,#5468,.T.);
#8225=ORIENTED_EDGE('',*,*,#5478,.T.);
#8226=ORIENTED_EDGE('',*,*,#5481,.T.);
#8227=ORIENTED_EDGE('',*,*,#5490,.T.);
#8228=ORIENTED_EDGE('',*,*,#5493,.T.);
#8229=ORIENTED_EDGE('',*,*,#5503,.T.);
#8230=ORIENTED_EDGE('',*,*,#5522,.T.);
#8231=ORIENTED_EDGE('',*,*,#5532,.T.);
#8232=ORIENTED_EDGE('',*,*,#5551,.T.);
#8233=ORIENTED_EDGE('',*,*,#5570,.T.);
#8234=ORIENTED_EDGE('',*,*,#5589,.T.);
#8235=ORIENTED_EDGE('',*,*,#5592,.T.);
#8236=ORIENTED_EDGE('',*,*,#5386,.T.);
#8237=ORIENTED_EDGE('',*,*,#5383,.T.);
#8238=ORIENTED_EDGE('',*,*,#5449,.T.);
#8239=ORIENTED_EDGE('',*,*,#5607,.F.);
#8240=ORIENTED_EDGE('',*,*,#5459,.T.);
#8241=ORIENTED_EDGE('',*,*,#5794,.F.);
#8242=ORIENTED_EDGE('',*,*,#5513,.T.);
#8243=ORIENTED_EDGE('',*,*,#5655,.F.);
#8244=ORIENTED_EDGE('',*,*,#5553,.T.);
#8245=ORIENTED_EDGE('',*,*,#5569,.T.);
#8246=ORIENTED_EDGE('',*,*,#5800,.F.);
#8247=ORIENTED_EDGE('',*,*,#5705,.F.);
#8248=ORIENTED_EDGE('',*,*,#5721,.F.);
#8249=ORIENTED_EDGE('',*,*,#5734,.F.);
#8250=ORIENTED_EDGE('',*,*,#5790,.F.);
#8251=ORIENTED_EDGE('',*,*,#5783,.F.);
#8252=ORIENTED_EDGE('',*,*,#5771,.F.);
#8253=ORIENTED_EDGE('',*,*,#5768,.F.);
#8254=ORIENTED_EDGE('',*,*,#5770,.F.);
#8255=ORIENTED_EDGE('',*,*,#5758,.F.);
#8256=ORIENTED_EDGE('',*,*,#5744,.F.);
#8257=ORIENTED_EDGE('',*,*,#5746,.F.);
#8258=ORIENTED_EDGE('',*,*,#5730,.F.);
#8259=ORIENTED_EDGE('',*,*,#5717,.F.);
#8260=ORIENTED_EDGE('',*,*,#5702,.F.);
#8261=ORIENTED_EDGE('',*,*,#5704,.F.);
#8262=ORIENTED_EDGE('',*,*,#5799,.F.);
#8263=ORIENTED_EDGE('',*,*,#5802,.T.);
#8264=ORIENTED_EDGE('',*,*,#5803,.T.);
#8265=ORIENTED_EDGE('',*,*,#5804,.T.);
#8266=ORIENTED_EDGE('',*,*,#5805,.T.);
#8267=ORIENTED_EDGE('',*,*,#5806,.T.);
#8268=ORIENTED_EDGE('',*,*,#5807,.T.);
#8269=ORIENTED_EDGE('',*,*,#5804,.F.);
#8270=ORIENTED_EDGE('',*,*,#5808,.T.);
#8271=ORIENTED_EDGE('',*,*,#5809,.T.);
#8272=ORIENTED_EDGE('',*,*,#5810,.T.);
#8273=ORIENTED_EDGE('',*,*,#5806,.F.);
#8274=ORIENTED_EDGE('',*,*,#5811,.T.);
#8275=ORIENTED_EDGE('',*,*,#5802,.F.);
#8276=ORIENTED_EDGE('',*,*,#5812,.T.);
#8277=ORIENTED_EDGE('',*,*,#5809,.F.);
#8278=ORIENTED_EDGE('',*,*,#5813,.T.);
#8279=ORIENTED_EDGE('',*,*,#5808,.F.);
#8280=ORIENTED_EDGE('',*,*,#5814,.F.);
#8281=ORIENTED_EDGE('',*,*,#5815,.F.);
#8282=ORIENTED_EDGE('',*,*,#5816,.T.);
#8283=ORIENTED_EDGE('',*,*,#5803,.F.);
#8284=ORIENTED_EDGE('',*,*,#5817,.F.);
#8285=ORIENTED_EDGE('',*,*,#5818,.F.);
#8286=ORIENTED_EDGE('',*,*,#5814,.T.);
#8287=ORIENTED_EDGE('',*,*,#5819,.F.);
#8288=ORIENTED_EDGE('',*,*,#5820,.F.);
#8289=ORIENTED_EDGE('',*,*,#5821,.F.);
#8290=ORIENTED_EDGE('',*,*,#5822,.F.);
#8291=ORIENTED_EDGE('',*,*,#5805,.F.);
#8292=ORIENTED_EDGE('',*,*,#5807,.F.);
#8293=ORIENTED_EDGE('',*,*,#5810,.F.);
#8294=ORIENTED_EDGE('',*,*,#5812,.F.);
#8295=ORIENTED_EDGE('',*,*,#5823,.F.);
#8296=ORIENTED_EDGE('',*,*,#5824,.F.);
#8297=ORIENTED_EDGE('',*,*,#5825,.F.);
#8298=ORIENTED_EDGE('',*,*,#5826,.T.);
#8299=ORIENTED_EDGE('',*,*,#5827,.F.);
#8300=ORIENTED_EDGE('',*,*,#5828,.F.);
#8301=ORIENTED_EDGE('',*,*,#5829,.F.);
#8302=ORIENTED_EDGE('',*,*,#5830,.T.);
#8303=ORIENTED_EDGE('',*,*,#5831,.F.);
#8304=ORIENTED_EDGE('',*,*,#5832,.F.);
#8305=ORIENTED_EDGE('',*,*,#5833,.F.);
#8306=ORIENTED_EDGE('',*,*,#5834,.T.);
#8307=ORIENTED_EDGE('',*,*,#5831,.T.);
#8308=ORIENTED_EDGE('',*,*,#5835,.T.);
#8309=ORIENTED_EDGE('',*,*,#5836,.T.);
#8310=ORIENTED_EDGE('',*,*,#5837,.F.);
#8311=ORIENTED_EDGE('',*,*,#5838,.F.);
#8312=ORIENTED_EDGE('',*,*,#5839,.F.);
#8313=ORIENTED_EDGE('',*,*,#5840,.F.);
#8314=ORIENTED_EDGE('',*,*,#5841,.F.);
#8315=ORIENTED_EDGE('',*,*,#5842,.F.);
#8316=ORIENTED_EDGE('',*,*,#5843,.T.);
#8317=ORIENTED_EDGE('',*,*,#5841,.T.);
#8318=ORIENTED_EDGE('',*,*,#5844,.T.);
#8319=ORIENTED_EDGE('',*,*,#5836,.F.);
#8320=ORIENTED_EDGE('',*,*,#5845,.F.);
#8321=ORIENTED_EDGE('',*,*,#5846,.F.);
#8322=ORIENTED_EDGE('',*,*,#5847,.F.);
#8323=ORIENTED_EDGE('',*,*,#5848,.F.);
#8324=ORIENTED_EDGE('',*,*,#5849,.F.);
#8325=ORIENTED_EDGE('',*,*,#5850,.F.);
#8326=ORIENTED_EDGE('',*,*,#5851,.F.);
#8327=ORIENTED_EDGE('',*,*,#5852,.F.);
#8328=ORIENTED_EDGE('',*,*,#5853,.F.);
#8329=ORIENTED_EDGE('',*,*,#5854,.F.);
#8330=ORIENTED_EDGE('',*,*,#5855,.F.);
#8331=ORIENTED_EDGE('',*,*,#5856,.F.);
#8332=ORIENTED_EDGE('',*,*,#5855,.T.);
#8333=ORIENTED_EDGE('',*,*,#5857,.T.);
#8334=ORIENTED_EDGE('',*,*,#5842,.T.);
#8335=ORIENTED_EDGE('',*,*,#5858,.T.);
#8336=ORIENTED_EDGE('',*,*,#5859,.F.);
#8337=ORIENTED_EDGE('',*,*,#5860,.F.);
#8338=ORIENTED_EDGE('',*,*,#5861,.F.);
#8339=ORIENTED_EDGE('',*,*,#5856,.T.);
#8340=ORIENTED_EDGE('',*,*,#5862,.T.);
#8341=ORIENTED_EDGE('',*,*,#5860,.T.);
#8342=ORIENTED_EDGE('',*,*,#5863,.T.);
#8343=ORIENTED_EDGE('',*,*,#5861,.T.);
#8344=ORIENTED_EDGE('',*,*,#5864,.T.);
#8345=ORIENTED_EDGE('',*,*,#5849,.T.);
#8346=ORIENTED_EDGE('',*,*,#5865,.T.);
#8347=ORIENTED_EDGE('',*,*,#5852,.T.);
#8348=ORIENTED_EDGE('',*,*,#5866,.T.);
#8349=ORIENTED_EDGE('',*,*,#5859,.T.);
#8350=ORIENTED_EDGE('',*,*,#5867,.T.);
#8351=ORIENTED_EDGE('',*,*,#5846,.T.);
#8352=ORIENTED_EDGE('',*,*,#5868,.T.);
#8353=ORIENTED_EDGE('',*,*,#5854,.T.);
#8354=ORIENTED_EDGE('',*,*,#5869,.T.);
#8355=ORIENTED_EDGE('',*,*,#5837,.T.);
#8356=ORIENTED_EDGE('',*,*,#5870,.T.);
#8357=ORIENTED_EDGE('',*,*,#5853,.T.);
#8358=ORIENTED_EDGE('',*,*,#5871,.T.);
#8359=ORIENTED_EDGE('',*,*,#5851,.T.);
#8360=ORIENTED_EDGE('',*,*,#5872,.T.);
#8361=ORIENTED_EDGE('',*,*,#5847,.T.);
#8362=ORIENTED_EDGE('',*,*,#5873,.T.);
#8363=ORIENTED_EDGE('',*,*,#5850,.T.);
#8364=ORIENTED_EDGE('',*,*,#5874,.T.);
#8365=ORIENTED_EDGE('',*,*,#5833,.T.);
#8366=ORIENTED_EDGE('',*,*,#5819,.T.);
#8367=ORIENTED_EDGE('',*,*,#5838,.T.);
#8368=ORIENTED_EDGE('',*,*,#5875,.T.);
#8369=ORIENTED_EDGE('',*,*,#5848,.T.);
#8370=ORIENTED_EDGE('',*,*,#5822,.T.);
#8371=ORIENTED_EDGE('',*,*,#5845,.T.);
#8372=ORIENTED_EDGE('',*,*,#5876,.T.);
#8373=ORIENTED_EDGE('',*,*,#5829,.T.);
#8374=ORIENTED_EDGE('',*,*,#5877,.T.);
#8375=ORIENTED_EDGE('',*,*,#5828,.T.);
#8376=ORIENTED_EDGE('',*,*,#5878,.T.);
#8377=ORIENTED_EDGE('',*,*,#5840,.T.);
#8378=ORIENTED_EDGE('',*,*,#5879,.T.);
#8379=ORIENTED_EDGE('',*,*,#5823,.T.);
#8380=ORIENTED_EDGE('',*,*,#5880,.T.);
#8381=ORIENTED_EDGE('',*,*,#5839,.T.);
#8382=ORIENTED_EDGE('',*,*,#5821,.T.);
#8383=ORIENTED_EDGE('',*,*,#5824,.T.);
#8384=ORIENTED_EDGE('',*,*,#5820,.T.);
#8385=ORIENTED_EDGE('',*,*,#5832,.T.);
#8386=ORIENTED_EDGE('',*,*,#5881,.T.);
#8387=ORIENTED_EDGE('',*,*,#5882,.T.);
#8388=ORIENTED_EDGE('',*,*,#5827,.T.);
#8389=ORIENTED_EDGE('',*,*,#5883,.T.);
#8390=ORIENTED_EDGE('',*,*,#5884,.T.);
#8391=ORIENTED_EDGE('',*,*,#5885,.T.);
#8392=ORIENTED_EDGE('',*,*,#5825,.T.);
#8393=ORIENTED_EDGE('',*,*,#5886,.T.);
#8394=ORIENTED_EDGE('',*,*,#5884,.F.);
#8395=ORIENTED_EDGE('',*,*,#5886,.F.);
#8396=ORIENTED_EDGE('',*,*,#5881,.F.);
#8397=ORIENTED_EDGE('',*,*,#5834,.F.);
#8398=ORIENTED_EDGE('',*,*,#5887,.T.);
#8399=ORIENTED_EDGE('',*,*,#5830,.F.);
#8400=ORIENTED_EDGE('',*,*,#5874,.F.);
#8401=ORIENTED_EDGE('',*,*,#5864,.F.);
#8402=ORIENTED_EDGE('',*,*,#5862,.F.);
#8403=ORIENTED_EDGE('',*,*,#5858,.F.);
#8404=ORIENTED_EDGE('',*,*,#5843,.F.);
#8405=ORIENTED_EDGE('',*,*,#5835,.F.);
#8406=ORIENTED_EDGE('',*,*,#5857,.F.);
#8407=ORIENTED_EDGE('',*,*,#5868,.F.);
#8408=ORIENTED_EDGE('',*,*,#5877,.F.);
#8409=ORIENTED_EDGE('',*,*,#5879,.F.);
#8410=ORIENTED_EDGE('',*,*,#5863,.F.);
#8411=ORIENTED_EDGE('',*,*,#5866,.F.);
#8412=ORIENTED_EDGE('',*,*,#5873,.F.);
#8413=ORIENTED_EDGE('',*,*,#5869,.F.);
#8414=ORIENTED_EDGE('',*,*,#5888,.F.);
#8415=ORIENTED_EDGE('',*,*,#5889,.F.);
#8416=ORIENTED_EDGE('',*,*,#5890,.F.);
#8417=ORIENTED_EDGE('',*,*,#5891,.F.);
#8418=ORIENTED_EDGE('',*,*,#5865,.F.);
#8419=ORIENTED_EDGE('',*,*,#5875,.F.);
#8420=ORIENTED_EDGE('',*,*,#5871,.F.);
#8421=ORIENTED_EDGE('',*,*,#5867,.F.);
#8422=ORIENTED_EDGE('',*,*,#5870,.F.);
#8423=ORIENTED_EDGE('',*,*,#5880,.F.);
#8424=ORIENTED_EDGE('',*,*,#5826,.F.);
#8425=ORIENTED_EDGE('',*,*,#5885,.F.);
#8426=ORIENTED_EDGE('',*,*,#5883,.F.);
#8427=ORIENTED_EDGE('',*,*,#5876,.F.);
#8428=ORIENTED_EDGE('',*,*,#5872,.F.);
#8429=ORIENTED_EDGE('',*,*,#5892,.T.);
#8430=ORIENTED_EDGE('',*,*,#5818,.T.);
#8431=ORIENTED_EDGE('',*,*,#5893,.T.);
#8432=ORIENTED_EDGE('',*,*,#5888,.T.);
#8433=ORIENTED_EDGE('',*,*,#5894,.T.);
#8434=ORIENTED_EDGE('',*,*,#5889,.T.);
#8435=ORIENTED_EDGE('',*,*,#5893,.F.);
#8436=ORIENTED_EDGE('',*,*,#5895,.T.);
#8437=ORIENTED_EDGE('',*,*,#5896,.T.);
#8438=ORIENTED_EDGE('',*,*,#5890,.T.);
#8439=ORIENTED_EDGE('',*,*,#5894,.F.);
#8440=ORIENTED_EDGE('',*,*,#5897,.T.);
#8441=ORIENTED_EDGE('',*,*,#5892,.F.);
#8442=ORIENTED_EDGE('',*,*,#5891,.T.);
#8443=ORIENTED_EDGE('',*,*,#5896,.F.);
#8444=ORIENTED_EDGE('',*,*,#5815,.T.);
#8445=ORIENTED_EDGE('',*,*,#5813,.F.);
#8446=ORIENTED_EDGE('',*,*,#5898,.F.);
#8447=ORIENTED_EDGE('',*,*,#5895,.F.);
#8448=ORIENTED_EDGE('',*,*,#5817,.T.);
#8449=ORIENTED_EDGE('',*,*,#5811,.F.);
#8450=ORIENTED_EDGE('',*,*,#5816,.F.);
#8451=ORIENTED_EDGE('',*,*,#5897,.F.);
#8452=ORIENTED_EDGE('',*,*,#5898,.T.);
#8453=ORIENTED_EDGE('',*,*,#5882,.F.);
#8454=ORIENTED_EDGE('',*,*,#5887,.F.);
#8455=ORIENTED_EDGE('',*,*,#5844,.F.);
#8456=ORIENTED_EDGE('',*,*,#5878,.F.);
#8457=ORIENTED_EDGE('',*,*,#5899,.F.);
#8458=ORIENTED_EDGE('',*,*,#5900,.T.);
#8459=ORIENTED_EDGE('',*,*,#5901,.T.);
#8460=ORIENTED_EDGE('',*,*,#5902,.T.);
#8461=ORIENTED_EDGE('',*,*,#5903,.T.);
#8462=ORIENTED_EDGE('',*,*,#5902,.F.);
#8463=ORIENTED_EDGE('',*,*,#5903,.F.);
#8464=ORIENTED_EDGE('',*,*,#5904,.T.);
#8465=ORIENTED_EDGE('',*,*,#5905,.F.);
#8466=ORIENTED_EDGE('',*,*,#5904,.F.);
#8467=ORIENTED_EDGE('',*,*,#5901,.F.);
#8468=ORIENTED_EDGE('',*,*,#5905,.T.);
#8469=ORIENTED_EDGE('',*,*,#5906,.T.);
#8470=ORIENTED_EDGE('',*,*,#5899,.T.);
#8471=ORIENTED_EDGE('',*,*,#5906,.F.);
#8472=ORIENTED_EDGE('',*,*,#5900,.F.);
#8473=ORIENTED_EDGE('',*,*,#5907,.T.);
#8474=ORIENTED_EDGE('',*,*,#5908,.T.);
#8475=ORIENTED_EDGE('',*,*,#5907,.F.);
#8476=ORIENTED_EDGE('',*,*,#5908,.F.);
#8477=ORIENTED_EDGE('',*,*,#5909,.F.);
#8478=ORIENTED_EDGE('',*,*,#5910,.F.);
#8479=ORIENTED_EDGE('',*,*,#5911,.F.);
#8480=ORIENTED_EDGE('',*,*,#5912,.F.);
#8481=ORIENTED_EDGE('',*,*,#5913,.F.);
#8482=ORIENTED_EDGE('',*,*,#5914,.F.);
#8483=ORIENTED_EDGE('',*,*,#5911,.T.);
#8484=ORIENTED_EDGE('',*,*,#5915,.F.);
#8485=ORIENTED_EDGE('',*,*,#5916,.F.);
#8486=ORIENTED_EDGE('',*,*,#5917,.F.);
#8487=ORIENTED_EDGE('',*,*,#5913,.T.);
#8488=ORIENTED_EDGE('',*,*,#5918,.F.);
#8489=ORIENTED_EDGE('',*,*,#5909,.T.);
#8490=ORIENTED_EDGE('',*,*,#5919,.F.);
#8491=ORIENTED_EDGE('',*,*,#5916,.T.);
#8492=ORIENTED_EDGE('',*,*,#5920,.F.);
#8493=ORIENTED_EDGE('',*,*,#5914,.T.);
#8494=ORIENTED_EDGE('',*,*,#5921,.F.);
#8495=ORIENTED_EDGE('',*,*,#5922,.T.);
#8496=ORIENTED_EDGE('',*,*,#5923,.T.);
#8497=ORIENTED_EDGE('',*,*,#5912,.T.);
#8498=ORIENTED_EDGE('',*,*,#5923,.F.);
#8499=ORIENTED_EDGE('',*,*,#5924,.T.);
#8500=ORIENTED_EDGE('',*,*,#5925,.T.);
#8501=ORIENTED_EDGE('',*,*,#5926,.T.);
#8502=ORIENTED_EDGE('',*,*,#5927,.T.);
#8503=ORIENTED_EDGE('',*,*,#5928,.T.);
#8504=ORIENTED_EDGE('',*,*,#5929,.T.);
#8505=ORIENTED_EDGE('',*,*,#5910,.T.);
#8506=ORIENTED_EDGE('',*,*,#5920,.T.);
#8507=ORIENTED_EDGE('',*,*,#5918,.T.);
#8508=ORIENTED_EDGE('',*,*,#5915,.T.);
#8509=ORIENTED_EDGE('',*,*,#5930,.T.);
#8510=ORIENTED_EDGE('',*,*,#5931,.F.);
#8511=ORIENTED_EDGE('',*,*,#5932,.T.);
#8512=ORIENTED_EDGE('',*,*,#5933,.T.);
#8513=ORIENTED_EDGE('',*,*,#5934,.T.);
#8514=ORIENTED_EDGE('',*,*,#5935,.T.);
#8515=ORIENTED_EDGE('',*,*,#5936,.T.);
#8516=ORIENTED_EDGE('',*,*,#5937,.F.);
#8517=ORIENTED_EDGE('',*,*,#5938,.T.);
#8518=ORIENTED_EDGE('',*,*,#5939,.T.);
#8519=ORIENTED_EDGE('',*,*,#5940,.T.);
#8520=ORIENTED_EDGE('',*,*,#5941,.F.);
#8521=ORIENTED_EDGE('',*,*,#5942,.F.);
#8522=ORIENTED_EDGE('',*,*,#5943,.F.);
#8523=ORIENTED_EDGE('',*,*,#5940,.F.);
#8524=ORIENTED_EDGE('',*,*,#5944,.T.);
#8525=ORIENTED_EDGE('',*,*,#5945,.T.);
#8526=ORIENTED_EDGE('',*,*,#5946,.T.);
#8527=ORIENTED_EDGE('',*,*,#5947,.T.);
#8528=ORIENTED_EDGE('',*,*,#5948,.T.);
#8529=ORIENTED_EDGE('',*,*,#5949,.T.);
#8530=ORIENTED_EDGE('',*,*,#5950,.F.);
#8531=ORIENTED_EDGE('',*,*,#5942,.T.);
#8532=ORIENTED_EDGE('',*,*,#5951,.F.);
#8533=ORIENTED_EDGE('',*,*,#5949,.F.);
#8534=ORIENTED_EDGE('',*,*,#5952,.T.);
#8535=ORIENTED_EDGE('',*,*,#5953,.T.);
#8536=ORIENTED_EDGE('',*,*,#5954,.T.);
#8537=ORIENTED_EDGE('',*,*,#5955,.T.);
#8538=ORIENTED_EDGE('',*,*,#5956,.T.);
#8539=ORIENTED_EDGE('',*,*,#5957,.T.);
#8540=ORIENTED_EDGE('',*,*,#5958,.T.);
#8541=ORIENTED_EDGE('',*,*,#5959,.T.);
#8542=ORIENTED_EDGE('',*,*,#5960,.T.);
#8543=ORIENTED_EDGE('',*,*,#5961,.T.);
#8544=ORIENTED_EDGE('',*,*,#5962,.T.);
#8545=ORIENTED_EDGE('',*,*,#5963,.T.);
#8546=ORIENTED_EDGE('',*,*,#5963,.F.);
#8547=ORIENTED_EDGE('',*,*,#5964,.F.);
#8548=ORIENTED_EDGE('',*,*,#5948,.F.);
#8549=ORIENTED_EDGE('',*,*,#5965,.F.);
#8550=ORIENTED_EDGE('',*,*,#5966,.T.);
#8551=ORIENTED_EDGE('',*,*,#5967,.T.);
#8552=ORIENTED_EDGE('',*,*,#5968,.T.);
#8553=ORIENTED_EDGE('',*,*,#5962,.F.);
#8554=ORIENTED_EDGE('',*,*,#5969,.F.);
#8555=ORIENTED_EDGE('',*,*,#5968,.F.);
#8556=ORIENTED_EDGE('',*,*,#5970,.F.);
#8557=ORIENTED_EDGE('',*,*,#5967,.F.);
#8558=ORIENTED_EDGE('',*,*,#5971,.F.);
#8559=ORIENTED_EDGE('',*,*,#5957,.F.);
#8560=ORIENTED_EDGE('',*,*,#5972,.F.);
#8561=ORIENTED_EDGE('',*,*,#5960,.F.);
#8562=ORIENTED_EDGE('',*,*,#5973,.F.);
#8563=ORIENTED_EDGE('',*,*,#5966,.F.);
#8564=ORIENTED_EDGE('',*,*,#5974,.F.);
#8565=ORIENTED_EDGE('',*,*,#5954,.F.);
#8566=ORIENTED_EDGE('',*,*,#5975,.F.);
#8567=ORIENTED_EDGE('',*,*,#5961,.F.);
#8568=ORIENTED_EDGE('',*,*,#5976,.F.);
#8569=ORIENTED_EDGE('',*,*,#5944,.F.);
#8570=ORIENTED_EDGE('',*,*,#5977,.F.);
#8571=ORIENTED_EDGE('',*,*,#5959,.F.);
#8572=ORIENTED_EDGE('',*,*,#5978,.F.);
#8573=ORIENTED_EDGE('',*,*,#5958,.F.);
#8574=ORIENTED_EDGE('',*,*,#5979,.F.);
#8575=ORIENTED_EDGE('',*,*,#5953,.F.);
#8576=ORIENTED_EDGE('',*,*,#5980,.F.);
#8577=ORIENTED_EDGE('',*,*,#5956,.F.);
#8578=ORIENTED_EDGE('',*,*,#5926,.F.);
#8579=ORIENTED_EDGE('',*,*,#5938,.F.);
#8580=ORIENTED_EDGE('',*,*,#5981,.F.);
#8581=ORIENTED_EDGE('',*,*,#5946,.F.);
#8582=ORIENTED_EDGE('',*,*,#5927,.F.);
#8583=ORIENTED_EDGE('',*,*,#5955,.F.);
#8584=ORIENTED_EDGE('',*,*,#5982,.F.);
#8585=ORIENTED_EDGE('',*,*,#5952,.F.);
#8586=ORIENTED_EDGE('',*,*,#5983,.F.);
#8587=ORIENTED_EDGE('',*,*,#5935,.F.);
#8588=ORIENTED_EDGE('',*,*,#5984,.F.);
#8589=ORIENTED_EDGE('',*,*,#5936,.F.);
#8590=ORIENTED_EDGE('',*,*,#5985,.F.);
#8591=ORIENTED_EDGE('',*,*,#5947,.F.);
#8592=ORIENTED_EDGE('',*,*,#5986,.F.);
#8593=ORIENTED_EDGE('',*,*,#5930,.F.);
#8594=ORIENTED_EDGE('',*,*,#5928,.F.);
#8595=ORIENTED_EDGE('',*,*,#5945,.F.);
#8596=ORIENTED_EDGE('',*,*,#5987,.F.);
#8597=ORIENTED_EDGE('',*,*,#5933,.F.);
#8598=ORIENTED_EDGE('',*,*,#5988,.F.);
#8599=ORIENTED_EDGE('',*,*,#5939,.F.);
#8600=ORIENTED_EDGE('',*,*,#5929,.F.);
#8601=ORIENTED_EDGE('',*,*,#5989,.F.);
#8602=ORIENTED_EDGE('',*,*,#5990,.F.);
#8603=ORIENTED_EDGE('',*,*,#5991,.F.);
#8604=ORIENTED_EDGE('',*,*,#5934,.F.);
#8605=ORIENTED_EDGE('',*,*,#5992,.F.);
#8606=ORIENTED_EDGE('',*,*,#5990,.T.);
#8607=ORIENTED_EDGE('',*,*,#5993,.F.);
#8608=ORIENTED_EDGE('',*,*,#5932,.F.);
#8609=ORIENTED_EDGE('',*,*,#5993,.T.);
#8610=ORIENTED_EDGE('',*,*,#5994,.F.);
#8611=ORIENTED_EDGE('',*,*,#5941,.T.);
#8612=ORIENTED_EDGE('',*,*,#5988,.T.);
#8613=ORIENTED_EDGE('',*,*,#5937,.T.);
#8614=ORIENTED_EDGE('',*,*,#5943,.T.);
#8615=ORIENTED_EDGE('',*,*,#5950,.T.);
#8616=ORIENTED_EDGE('',*,*,#5964,.T.);
#8617=ORIENTED_EDGE('',*,*,#5970,.T.);
#8618=ORIENTED_EDGE('',*,*,#5972,.T.);
#8619=ORIENTED_EDGE('',*,*,#5981,.T.);
#8620=ORIENTED_EDGE('',*,*,#5965,.T.);
#8621=ORIENTED_EDGE('',*,*,#5985,.T.);
#8622=ORIENTED_EDGE('',*,*,#5983,.T.);
#8623=ORIENTED_EDGE('',*,*,#5976,.T.);
#8624=ORIENTED_EDGE('',*,*,#5969,.T.);
#8625=ORIENTED_EDGE('',*,*,#5975,.T.);
#8626=ORIENTED_EDGE('',*,*,#5979,.T.);
#8627=ORIENTED_EDGE('',*,*,#5974,.T.);
#8628=ORIENTED_EDGE('',*,*,#5995,.T.);
#8629=ORIENTED_EDGE('',*,*,#5996,.T.);
#8630=ORIENTED_EDGE('',*,*,#5997,.T.);
#8631=ORIENTED_EDGE('',*,*,#5998,.T.);
#8632=ORIENTED_EDGE('',*,*,#5971,.T.);
#8633=ORIENTED_EDGE('',*,*,#5973,.T.);
#8634=ORIENTED_EDGE('',*,*,#5977,.T.);
#8635=ORIENTED_EDGE('',*,*,#5982,.T.);
#8636=ORIENTED_EDGE('',*,*,#5978,.T.);
#8637=ORIENTED_EDGE('',*,*,#5980,.T.);
#8638=ORIENTED_EDGE('',*,*,#5984,.T.);
#8639=ORIENTED_EDGE('',*,*,#5991,.T.);
#8640=ORIENTED_EDGE('',*,*,#5992,.T.);
#8641=ORIENTED_EDGE('',*,*,#5931,.T.);
#8642=ORIENTED_EDGE('',*,*,#5987,.T.);
#8643=ORIENTED_EDGE('',*,*,#5999,.F.);
#8644=ORIENTED_EDGE('',*,*,#5995,.F.);
#8645=ORIENTED_EDGE('',*,*,#6000,.F.);
#8646=ORIENTED_EDGE('',*,*,#5924,.F.);
#8647=ORIENTED_EDGE('',*,*,#6001,.F.);
#8648=ORIENTED_EDGE('',*,*,#6002,.F.);
#8649=ORIENTED_EDGE('',*,*,#6000,.T.);
#8650=ORIENTED_EDGE('',*,*,#5998,.F.);
#8651=ORIENTED_EDGE('',*,*,#6003,.F.);
#8652=ORIENTED_EDGE('',*,*,#6004,.F.);
#8653=ORIENTED_EDGE('',*,*,#6001,.T.);
#8654=ORIENTED_EDGE('',*,*,#5997,.F.);
#8655=ORIENTED_EDGE('',*,*,#5999,.T.);
#8656=ORIENTED_EDGE('',*,*,#5922,.F.);
#8657=ORIENTED_EDGE('',*,*,#6003,.T.);
#8658=ORIENTED_EDGE('',*,*,#5996,.F.);
#8659=ORIENTED_EDGE('',*,*,#5919,.T.);
#8660=ORIENTED_EDGE('',*,*,#5925,.F.);
#8661=ORIENTED_EDGE('',*,*,#6002,.T.);
#8662=ORIENTED_EDGE('',*,*,#6005,.T.);
#8663=ORIENTED_EDGE('',*,*,#5917,.T.);
#8664=ORIENTED_EDGE('',*,*,#6005,.F.);
#8665=ORIENTED_EDGE('',*,*,#6004,.T.);
#8666=ORIENTED_EDGE('',*,*,#5921,.T.);
#8667=ORIENTED_EDGE('',*,*,#5989,.T.);
#8668=ORIENTED_EDGE('',*,*,#5986,.T.);
#8669=ORIENTED_EDGE('',*,*,#5951,.T.);
#8670=ORIENTED_EDGE('',*,*,#5994,.T.);
#8671=ORIENTED_EDGE('',*,*,#6006,.T.);
#8672=ORIENTED_EDGE('',*,*,#6007,.T.);
#8673=ORIENTED_EDGE('',*,*,#6008,.T.);
#8674=ORIENTED_EDGE('',*,*,#6009,.T.);
#8675=ORIENTED_EDGE('',*,*,#6010,.T.);
#8676=ORIENTED_EDGE('',*,*,#6011,.T.);
#8677=ORIENTED_EDGE('',*,*,#6008,.F.);
#8678=ORIENTED_EDGE('',*,*,#6012,.T.);
#8679=ORIENTED_EDGE('',*,*,#6013,.T.);
#8680=ORIENTED_EDGE('',*,*,#6014,.T.);
#8681=ORIENTED_EDGE('',*,*,#6010,.F.);
#8682=ORIENTED_EDGE('',*,*,#6015,.T.);
#8683=ORIENTED_EDGE('',*,*,#6006,.F.);
#8684=ORIENTED_EDGE('',*,*,#6016,.T.);
#8685=ORIENTED_EDGE('',*,*,#6013,.F.);
#8686=ORIENTED_EDGE('',*,*,#6017,.T.);
#8687=ORIENTED_EDGE('',*,*,#6012,.F.);
#8688=ORIENTED_EDGE('',*,*,#6018,.F.);
#8689=ORIENTED_EDGE('',*,*,#6019,.F.);
#8690=ORIENTED_EDGE('',*,*,#6020,.T.);
#8691=ORIENTED_EDGE('',*,*,#6007,.F.);
#8692=ORIENTED_EDGE('',*,*,#6021,.F.);
#8693=ORIENTED_EDGE('',*,*,#6022,.F.);
#8694=ORIENTED_EDGE('',*,*,#6018,.T.);
#8695=ORIENTED_EDGE('',*,*,#6023,.F.);
#8696=ORIENTED_EDGE('',*,*,#6024,.F.);
#8697=ORIENTED_EDGE('',*,*,#6025,.F.);
#8698=ORIENTED_EDGE('',*,*,#6026,.F.);
#8699=ORIENTED_EDGE('',*,*,#6009,.F.);
#8700=ORIENTED_EDGE('',*,*,#6011,.F.);
#8701=ORIENTED_EDGE('',*,*,#6014,.F.);
#8702=ORIENTED_EDGE('',*,*,#6016,.F.);
#8703=ORIENTED_EDGE('',*,*,#6027,.F.);
#8704=ORIENTED_EDGE('',*,*,#6028,.F.);
#8705=ORIENTED_EDGE('',*,*,#6029,.F.);
#8706=ORIENTED_EDGE('',*,*,#6030,.T.);
#8707=ORIENTED_EDGE('',*,*,#6031,.F.);
#8708=ORIENTED_EDGE('',*,*,#6032,.F.);
#8709=ORIENTED_EDGE('',*,*,#6033,.F.);
#8710=ORIENTED_EDGE('',*,*,#6034,.T.);
#8711=ORIENTED_EDGE('',*,*,#6035,.F.);
#8712=ORIENTED_EDGE('',*,*,#6036,.F.);
#8713=ORIENTED_EDGE('',*,*,#6037,.F.);
#8714=ORIENTED_EDGE('',*,*,#6038,.T.);
#8715=ORIENTED_EDGE('',*,*,#6035,.T.);
#8716=ORIENTED_EDGE('',*,*,#6039,.T.);
#8717=ORIENTED_EDGE('',*,*,#6040,.T.);
#8718=ORIENTED_EDGE('',*,*,#6041,.F.);
#8719=ORIENTED_EDGE('',*,*,#6042,.F.);
#8720=ORIENTED_EDGE('',*,*,#6043,.F.);
#8721=ORIENTED_EDGE('',*,*,#6044,.F.);
#8722=ORIENTED_EDGE('',*,*,#6045,.F.);
#8723=ORIENTED_EDGE('',*,*,#6046,.F.);
#8724=ORIENTED_EDGE('',*,*,#6047,.T.);
#8725=ORIENTED_EDGE('',*,*,#6045,.T.);
#8726=ORIENTED_EDGE('',*,*,#6048,.T.);
#8727=ORIENTED_EDGE('',*,*,#6040,.F.);
#8728=ORIENTED_EDGE('',*,*,#6049,.F.);
#8729=ORIENTED_EDGE('',*,*,#6050,.F.);
#8730=ORIENTED_EDGE('',*,*,#6051,.F.);
#8731=ORIENTED_EDGE('',*,*,#6052,.F.);
#8732=ORIENTED_EDGE('',*,*,#6053,.F.);
#8733=ORIENTED_EDGE('',*,*,#6054,.F.);
#8734=ORIENTED_EDGE('',*,*,#6055,.F.);
#8735=ORIENTED_EDGE('',*,*,#6056,.F.);
#8736=ORIENTED_EDGE('',*,*,#6057,.F.);
#8737=ORIENTED_EDGE('',*,*,#6058,.F.);
#8738=ORIENTED_EDGE('',*,*,#6059,.F.);
#8739=ORIENTED_EDGE('',*,*,#6060,.F.);
#8740=ORIENTED_EDGE('',*,*,#6059,.T.);
#8741=ORIENTED_EDGE('',*,*,#6061,.T.);
#8742=ORIENTED_EDGE('',*,*,#6046,.T.);
#8743=ORIENTED_EDGE('',*,*,#6062,.T.);
#8744=ORIENTED_EDGE('',*,*,#6063,.F.);
#8745=ORIENTED_EDGE('',*,*,#6064,.F.);
#8746=ORIENTED_EDGE('',*,*,#6065,.F.);
#8747=ORIENTED_EDGE('',*,*,#6060,.T.);
#8748=ORIENTED_EDGE('',*,*,#6066,.T.);
#8749=ORIENTED_EDGE('',*,*,#6064,.T.);
#8750=ORIENTED_EDGE('',*,*,#6067,.T.);
#8751=ORIENTED_EDGE('',*,*,#6065,.T.);
#8752=ORIENTED_EDGE('',*,*,#6068,.T.);
#8753=ORIENTED_EDGE('',*,*,#6053,.T.);
#8754=ORIENTED_EDGE('',*,*,#6069,.T.);
#8755=ORIENTED_EDGE('',*,*,#6056,.T.);
#8756=ORIENTED_EDGE('',*,*,#6070,.T.);
#8757=ORIENTED_EDGE('',*,*,#6063,.T.);
#8758=ORIENTED_EDGE('',*,*,#6071,.T.);
#8759=ORIENTED_EDGE('',*,*,#6050,.T.);
#8760=ORIENTED_EDGE('',*,*,#6072,.T.);
#8761=ORIENTED_EDGE('',*,*,#6058,.T.);
#8762=ORIENTED_EDGE('',*,*,#6073,.T.);
#8763=ORIENTED_EDGE('',*,*,#6041,.T.);
#8764=ORIENTED_EDGE('',*,*,#6074,.T.);
#8765=ORIENTED_EDGE('',*,*,#6057,.T.);
#8766=ORIENTED_EDGE('',*,*,#6075,.T.);
#8767=ORIENTED_EDGE('',*,*,#6055,.T.);
#8768=ORIENTED_EDGE('',*,*,#6076,.T.);
#8769=ORIENTED_EDGE('',*,*,#6051,.T.);
#8770=ORIENTED_EDGE('',*,*,#6077,.T.);
#8771=ORIENTED_EDGE('',*,*,#6054,.T.);
#8772=ORIENTED_EDGE('',*,*,#6078,.T.);
#8773=ORIENTED_EDGE('',*,*,#6037,.T.);
#8774=ORIENTED_EDGE('',*,*,#6023,.T.);
#8775=ORIENTED_EDGE('',*,*,#6042,.T.);
#8776=ORIENTED_EDGE('',*,*,#6079,.T.);
#8777=ORIENTED_EDGE('',*,*,#6052,.T.);
#8778=ORIENTED_EDGE('',*,*,#6026,.T.);
#8779=ORIENTED_EDGE('',*,*,#6049,.T.);
#8780=ORIENTED_EDGE('',*,*,#6080,.T.);
#8781=ORIENTED_EDGE('',*,*,#6033,.T.);
#8782=ORIENTED_EDGE('',*,*,#6081,.T.);
#8783=ORIENTED_EDGE('',*,*,#6032,.T.);
#8784=ORIENTED_EDGE('',*,*,#6082,.T.);
#8785=ORIENTED_EDGE('',*,*,#6044,.T.);
#8786=ORIENTED_EDGE('',*,*,#6083,.T.);
#8787=ORIENTED_EDGE('',*,*,#6027,.T.);
#8788=ORIENTED_EDGE('',*,*,#6084,.T.);
#8789=ORIENTED_EDGE('',*,*,#6043,.T.);
#8790=ORIENTED_EDGE('',*,*,#6025,.T.);
#8791=ORIENTED_EDGE('',*,*,#6028,.T.);
#8792=ORIENTED_EDGE('',*,*,#6024,.T.);
#8793=ORIENTED_EDGE('',*,*,#6036,.T.);
#8794=ORIENTED_EDGE('',*,*,#6085,.T.);
#8795=ORIENTED_EDGE('',*,*,#6086,.T.);
#8796=ORIENTED_EDGE('',*,*,#6031,.T.);
#8797=ORIENTED_EDGE('',*,*,#6087,.T.);
#8798=ORIENTED_EDGE('',*,*,#6088,.T.);
#8799=ORIENTED_EDGE('',*,*,#6089,.T.);
#8800=ORIENTED_EDGE('',*,*,#6029,.T.);
#8801=ORIENTED_EDGE('',*,*,#6090,.T.);
#8802=ORIENTED_EDGE('',*,*,#6088,.F.);
#8803=ORIENTED_EDGE('',*,*,#6090,.F.);
#8804=ORIENTED_EDGE('',*,*,#6085,.F.);
#8805=ORIENTED_EDGE('',*,*,#6038,.F.);
#8806=ORIENTED_EDGE('',*,*,#6091,.T.);
#8807=ORIENTED_EDGE('',*,*,#6034,.F.);
#8808=ORIENTED_EDGE('',*,*,#6078,.F.);
#8809=ORIENTED_EDGE('',*,*,#6068,.F.);
#8810=ORIENTED_EDGE('',*,*,#6066,.F.);
#8811=ORIENTED_EDGE('',*,*,#6062,.F.);
#8812=ORIENTED_EDGE('',*,*,#6047,.F.);
#8813=ORIENTED_EDGE('',*,*,#6039,.F.);
#8814=ORIENTED_EDGE('',*,*,#6061,.F.);
#8815=ORIENTED_EDGE('',*,*,#6072,.F.);
#8816=ORIENTED_EDGE('',*,*,#6081,.F.);
#8817=ORIENTED_EDGE('',*,*,#6083,.F.);
#8818=ORIENTED_EDGE('',*,*,#6067,.F.);
#8819=ORIENTED_EDGE('',*,*,#6070,.F.);
#8820=ORIENTED_EDGE('',*,*,#6077,.F.);
#8821=ORIENTED_EDGE('',*,*,#6073,.F.);
#8822=ORIENTED_EDGE('',*,*,#6092,.F.);
#8823=ORIENTED_EDGE('',*,*,#6093,.F.);
#8824=ORIENTED_EDGE('',*,*,#6094,.F.);
#8825=ORIENTED_EDGE('',*,*,#6095,.F.);
#8826=ORIENTED_EDGE('',*,*,#6069,.F.);
#8827=ORIENTED_EDGE('',*,*,#6079,.F.);
#8828=ORIENTED_EDGE('',*,*,#6075,.F.);
#8829=ORIENTED_EDGE('',*,*,#6071,.F.);
#8830=ORIENTED_EDGE('',*,*,#6074,.F.);
#8831=ORIENTED_EDGE('',*,*,#6084,.F.);
#8832=ORIENTED_EDGE('',*,*,#6030,.F.);
#8833=ORIENTED_EDGE('',*,*,#6089,.F.);
#8834=ORIENTED_EDGE('',*,*,#6087,.F.);
#8835=ORIENTED_EDGE('',*,*,#6080,.F.);
#8836=ORIENTED_EDGE('',*,*,#6076,.F.);
#8837=ORIENTED_EDGE('',*,*,#6096,.T.);
#8838=ORIENTED_EDGE('',*,*,#6022,.T.);
#8839=ORIENTED_EDGE('',*,*,#6097,.T.);
#8840=ORIENTED_EDGE('',*,*,#6092,.T.);
#8841=ORIENTED_EDGE('',*,*,#6098,.T.);
#8842=ORIENTED_EDGE('',*,*,#6093,.T.);
#8843=ORIENTED_EDGE('',*,*,#6097,.F.);
#8844=ORIENTED_EDGE('',*,*,#6099,.T.);
#8845=ORIENTED_EDGE('',*,*,#6100,.T.);
#8846=ORIENTED_EDGE('',*,*,#6094,.T.);
#8847=ORIENTED_EDGE('',*,*,#6098,.F.);
#8848=ORIENTED_EDGE('',*,*,#6101,.T.);
#8849=ORIENTED_EDGE('',*,*,#6096,.F.);
#8850=ORIENTED_EDGE('',*,*,#6095,.T.);
#8851=ORIENTED_EDGE('',*,*,#6100,.F.);
#8852=ORIENTED_EDGE('',*,*,#6019,.T.);
#8853=ORIENTED_EDGE('',*,*,#6017,.F.);
#8854=ORIENTED_EDGE('',*,*,#6102,.F.);
#8855=ORIENTED_EDGE('',*,*,#6099,.F.);
#8856=ORIENTED_EDGE('',*,*,#6021,.T.);
#8857=ORIENTED_EDGE('',*,*,#6015,.F.);
#8858=ORIENTED_EDGE('',*,*,#6020,.F.);
#8859=ORIENTED_EDGE('',*,*,#6101,.F.);
#8860=ORIENTED_EDGE('',*,*,#6102,.T.);
#8861=ORIENTED_EDGE('',*,*,#6086,.F.);
#8862=ORIENTED_EDGE('',*,*,#6091,.F.);
#8863=ORIENTED_EDGE('',*,*,#6048,.F.);
#8864=ORIENTED_EDGE('',*,*,#6082,.F.);
#8865=PLANE('',#9751);
#8866=PLANE('',#9759);
#8867=PLANE('',#9763);
#8868=PLANE('',#9765);
#8869=PLANE('',#9768);
#8870=PLANE('',#9771);
#8871=PLANE('',#9776);
#8872=PLANE('',#9777);
#8873=PLANE('',#9782);
#8874=PLANE('',#9787);
#8875=PLANE('',#9790);
#8876=PLANE('',#9793);
#8877=PLANE('',#9796);
#8878=PLANE('',#9801);
#8879=PLANE('',#9921);
#8880=PLANE('',#9922);
#8881=PLANE('',#9923);
#8882=PLANE('',#9924);
#8883=PLANE('',#9925);
#8884=PLANE('',#9926);
#8885=PLANE('',#9927);
#8886=PLANE('',#9928);
#8887=PLANE('',#9929);
#8888=PLANE('',#9930);
#8889=PLANE('',#9931);
#8890=PLANE('',#9939);
#8891=PLANE('',#9943);
#8892=PLANE('',#10087);
#8893=PLANE('',#10088);
#8894=PLANE('',#10089);
#8895=PLANE('',#10090);
#8896=PLANE('',#10091);
#8897=PLANE('',#10092);
#8898=PLANE('',#10093);
#8899=PLANE('',#10094);
#8900=PLANE('',#10095);
#8901=PLANE('',#10096);
#8902=PLANE('',#10097);
#8903=PLANE('',#10098);
#8904=PLANE('',#10099);
#8905=PLANE('',#10100);
#8906=PLANE('',#10105);
#8907=PLANE('',#10109);
#8908=PLANE('',#10113);
#8909=PLANE('',#10117);
#8910=PLANE('',#10121);
#8911=PLANE('',#10125);
#8912=PLANE('',#10129);
#8913=PLANE('',#10133);
#8914=PLANE('',#10134);
#8915=PLANE('',#10137);
#8916=PLANE('',#10140);
#8917=PLANE('',#10145);
#8918=PLANE('',#10146);
#8919=PLANE('',#10151);
#8920=PLANE('',#10156);
#8921=PLANE('',#10159);
#8922=PLANE('',#10162);
#8923=PLANE('',#10165);
#8924=PLANE('',#10170);
#8925=PLANE('',#10290);
#8926=PLANE('',#10291);
#8927=PLANE('',#10292);
#8928=PLANE('',#10293);
#8929=PLANE('',#10294);
#8930=PLANE('',#10295);
#8931=PLANE('',#10296);
#8932=PLANE('',#10297);
#8933=PLANE('',#10298);
#8934=PLANE('',#10299);
#8935=PLANE('',#10300);
#8936=PLANE('',#10316);
#8937=PLANE('',#10317);
#8938=PLANE('',#10379);
#8939=PLANE('',#10380);
#8940=PLANE('',#10381);
#8941=PLANE('',#10382);
#8942=PLANE('',#10385);
#8943=PLANE('',#10386);
#8944=PLANE('',#10397);
#8945=PLANE('',#10398);
#8946=PLANE('',#10408);
#8947=PLANE('',#10422);
#8948=PLANE('',#10518);
#8949=PLANE('',#10519);
#8950=PLANE('',#10520);
#8951=PLANE('',#10521);
#8952=PLANE('',#10535);
#8953=PLANE('',#10536);
#8954=PLANE('',#10537);
#8955=PLANE('',#10538);
#8956=PLANE('',#10539);
#8957=PLANE('',#10553);
#8958=PLANE('',#10554);
#8959=PLANE('',#10555);
#8960=PLANE('',#10556);
#8961=PLANE('',#10557);
#8962=PLANE('',#10558);
#8963=PLANE('',#10559);
#8964=PLANE('',#10560);
#8965=PLANE('',#10567);
#8966=PLANE('',#10574);
#8967=PLANE('',#10575);
#8968=PLANE('',#10576);
#8969=PLANE('',#10577);
#8970=PLANE('',#10583);
#8971=PLANE('',#10584);
#8972=PLANE('',#10705);
#8973=PLANE('',#10706);
#8974=PLANE('',#10707);
#8975=PLANE('',#10708);
#8976=PLANE('',#10709);
#8977=PLANE('',#10710);
#8978=PLANE('',#10711);
#8979=PLANE('',#10712);
#8980=PLANE('',#10713);
#8981=PLANE('',#10729);
#8982=PLANE('',#10730);
#8983=PLANE('',#10792);
#8984=PLANE('',#10793);
#8985=PLANE('',#10794);
#8986=PLANE('',#10795);
#8987=PLANE('',#10798);
#8988=PLANE('',#10799);
#8989=PLANE('',#10810);
#8990=PLANE('',#10811);
#8991=PLANE('',#10813);
#8992=PLANE('',#10821);
#8993=PLANE('',#10825);
#8994=PLANE('',#10841);
#8995=PLANE('',#10842);
#8996=PLANE('',#10904);
#8997=PLANE('',#10905);
#8998=PLANE('',#10906);
#8999=PLANE('',#10907);
#9000=PLANE('',#10910);
#9001=PLANE('',#10911);
#9002=PLANE('',#10922);
#9003=PLANE('',#10923);
#9004=PLANE('',#10939);
#9005=PLANE('',#10940);
#9006=PLANE('',#11002);
#9007=PLANE('',#11003);
#9008=PLANE('',#11004);
#9009=PLANE('',#11005);
#9010=PLANE('',#11008);
#9011=PLANE('',#11009);
#9012=PLANE('',#11020);
#9013=PLANE('',#11021);
#9014=ADVANCED_FACE('',(#2027,#1974),#8865,.F.);
#9015=ADVANCED_FACE('',(#2028),#1970,.T.);
#9016=ADVANCED_FACE('',(#2029),#327,.T.);
#9017=ADVANCED_FACE('',(#2030),#8866,.T.);
#9018=ADVANCED_FACE('',(#2031),#1971,.T.);
#9019=ADVANCED_FACE('',(#2032),#328,.T.);
#9020=ADVANCED_FACE('',(#2033),#8867,.F.);
#9021=ADVANCED_FACE('',(#2034),#8868,.T.);
#9022=ADVANCED_FACE('',(#2035),#8869,.T.);
#9023=ADVANCED_FACE('',(#2036),#8870,.T.);
#9024=ADVANCED_FACE('',(#2037),#329,.T.);
#9025=ADVANCED_FACE('',(#2038),#330,.T.);
#9026=ADVANCED_FACE('',(#2039),#8871,.T.);
#9027=ADVANCED_FACE('',(#2040),#8872,.T.);
#9028=ADVANCED_FACE('',(#2041),#331,.T.);
#9029=ADVANCED_FACE('',(#2042),#332,.T.);
#9030=ADVANCED_FACE('',(#2043),#8873,.T.);
#9031=ADVANCED_FACE('',(#2044),#8874,.F.);
#9032=ADVANCED_FACE('',(#2045),#8875,.F.);
#9033=ADVANCED_FACE('',(#2046),#8876,.F.);
#9034=ADVANCED_FACE('',(#2047),#333,.T.);
#9035=ADVANCED_FACE('',(#2048),#8877,.T.);
#9036=ADVANCED_FACE('',(#2049),#8878,.T.);
#9037=ADVANCED_FACE('',(#2050),#334,.T.);
#9038=ADVANCED_FACE('',(#2051),#211,.T.);
#9039=ADVANCED_FACE('',(#2052),#212,.T.);
#9040=ADVANCED_FACE('',(#2053),#119,.T.);
#9041=ADVANCED_FACE('',(#2054),#120,.T.);
#9042=ADVANCED_FACE('',(#2055),#335,.T.);
#9043=ADVANCED_FACE('',(#2056),#121,.T.);
#9044=ADVANCED_FACE('',(#2057),#336,.T.);
#9045=ADVANCED_FACE('',(#2058),#337,.T.);
#9046=ADVANCED_FACE('',(#2059),#122,.T.);
#9047=ADVANCED_FACE('',(#2060),#338,.T.);
#9048=ADVANCED_FACE('',(#2061),#339,.T.);
#9049=ADVANCED_FACE('',(#2062),#213,.T.);
#9050=ADVANCED_FACE('',(#2063),#123,.T.);
#9051=ADVANCED_FACE('',(#2064),#214,.T.);
#9052=ADVANCED_FACE('',(#2065),#340,.T.);
#9053=ADVANCED_FACE('',(#2066),#341,.F.);
#9054=ADVANCED_FACE('',(#2067),#124,.T.);
#9055=ADVANCED_FACE('',(#2068),#215,.T.);
#9056=ADVANCED_FACE('',(#2069),#216,.T.);
#9057=ADVANCED_FACE('',(#2070),#342,.T.);
#9058=ADVANCED_FACE('',(#2071),#343,.F.);
#9059=ADVANCED_FACE('',(#2072),#125,.T.);
#9060=ADVANCED_FACE('',(#2073),#126,.T.);
#9061=ADVANCED_FACE('',(#2074),#344,.T.);
#9062=ADVANCED_FACE('',(#2075),#127,.T.);
#9063=ADVANCED_FACE('',(#2076),#345,.T.);
#9064=ADVANCED_FACE('',(#2077),#346,.T.);
#9065=ADVANCED_FACE('',(#2078),#128,.T.);
#9066=ADVANCED_FACE('',(#2079),#347,.T.);
#9067=ADVANCED_FACE('',(#2080),#348,.T.);
#9068=ADVANCED_FACE('',(#2081),#217,.T.);
#9069=ADVANCED_FACE('',(#2082),#129,.T.);
#9070=ADVANCED_FACE('',(#2083),#349,.T.);
#9071=ADVANCED_FACE('',(#2084),#218,.T.);
#9072=ADVANCED_FACE('',(#2085),#130,.T.);
#9073=ADVANCED_FACE('',(#2086),#350,.T.);
#9074=ADVANCED_FACE('',(#2087),#131,.T.);
#9075=ADVANCED_FACE('',(#2088),#351,.T.);
#9076=ADVANCED_FACE('',(#2089),#352,.T.);
#9077=ADVANCED_FACE('',(#2090),#132,.T.);
#9078=ADVANCED_FACE('',(#2091),#353,.T.);
#9079=ADVANCED_FACE('',(#2092),#354,.T.);
#9080=ADVANCED_FACE('',(#2093),#355,.T.);
#9081=ADVANCED_FACE('',(#2094),#356,.T.);
#9082=ADVANCED_FACE('',(#2095),#357,.T.);
#9083=ADVANCED_FACE('',(#2096),#358,.F.);
#9084=ADVANCED_FACE('',(#2097),#359,.T.);
#9085=ADVANCED_FACE('',(#2098),#360,.T.);
#9086=ADVANCED_FACE('',(#2099),#361,.T.);
#9087=ADVANCED_FACE('',(#2100),#362,.T.);
#9088=ADVANCED_FACE('',(#2101),#363,.T.);
#9089=ADVANCED_FACE('',(#2102),#364,.T.);
#9090=ADVANCED_FACE('',(#2103),#365,.T.);
#9091=ADVANCED_FACE('',(#2104),#366,.T.);
#9092=ADVANCED_FACE('',(#2105),#367,.F.);
#9093=ADVANCED_FACE('',(#2106),#8879,.F.);
#9094=ADVANCED_FACE('',(#2107),#8880,.F.);
#9095=ADVANCED_FACE('',(#2108),#8881,.F.);
#9096=ADVANCED_FACE('',(#2109),#8882,.F.);
#9097=ADVANCED_FACE('',(#2110),#8883,.F.);
#9098=ADVANCED_FACE('',(#2111),#8884,.F.);
#9099=ADVANCED_FACE('',(#2112),#8885,.F.);
#9100=ADVANCED_FACE('',(#2113),#8886,.T.);
#9101=ADVANCED_FACE('',(#2114),#8887,.F.);
#9102=ADVANCED_FACE('',(#2115),#8888,.T.);
#9103=ADVANCED_FACE('',(#2116),#8889,.T.);
#9104=ADVANCED_FACE('',(#2117),#368,.F.);
#9105=ADVANCED_FACE('',(#2118),#369,.F.);
#9106=ADVANCED_FACE('',(#2119),#8890,.T.);
#9107=ADVANCED_FACE('',(#2120),#370,.F.);
#9108=ADVANCED_FACE('',(#2121),#8891,.T.);
#9109=ADVANCED_FACE('',(#2122),#371,.F.);
#9110=ADVANCED_FACE('',(#2123),#133,.T.);
#9111=ADVANCED_FACE('',(#2124),#134,.T.);
#9112=ADVANCED_FACE('',(#2125),#219,.T.);
#9113=ADVANCED_FACE('',(#2126),#372,.T.);
#9114=ADVANCED_FACE('',(#2127),#220,.T.);
#9115=ADVANCED_FACE('',(#2128),#221,.T.);
#9116=ADVANCED_FACE('',(#2129),#222,.T.);
#9117=ADVANCED_FACE('',(#2130),#373,.T.);
#9118=ADVANCED_FACE('',(#2131),#135,.T.);
#9119=ADVANCED_FACE('',(#2132),#374,.T.);
#9120=ADVANCED_FACE('',(#2133),#136,.T.);
#9121=ADVANCED_FACE('',(#2134),#375,.T.);
#9122=ADVANCED_FACE('',(#2135),#137,.T.);
#9123=ADVANCED_FACE('',(#2136),#138,.T.);
#9124=ADVANCED_FACE('',(#2137),#376,.T.);
#9125=ADVANCED_FACE('',(#2138),#139,.T.);
#9126=ADVANCED_FACE('',(#2139),#377,.T.);
#9127=ADVANCED_FACE('',(#2140),#140,.T.);
#9128=ADVANCED_FACE('',(#2141),#378,.T.);
#9129=ADVANCED_FACE('',(#2142),#141,.T.);
#9130=ADVANCED_FACE('',(#2143),#142,.T.);
#9131=ADVANCED_FACE('',(#2144),#379,.T.);
#9132=ADVANCED_FACE('',(#2145),#223,.T.);
#9133=ADVANCED_FACE('',(#2146),#380,.T.);
#9134=ADVANCED_FACE('',(#2147),#143,.T.);
#9135=ADVANCED_FACE('',(#2148),#224,.T.);
#9136=ADVANCED_FACE('',(#2149),#144,.T.);
#9137=ADVANCED_FACE('',(#2150),#145,.T.);
#9138=ADVANCED_FACE('',(#2151),#381,.T.);
#9139=ADVANCED_FACE('',(#2152),#146,.T.);
#9140=ADVANCED_FACE('',(#2153),#147,.T.);
#9141=ADVANCED_FACE('',(#2154),#148,.T.);
#9142=ADVANCED_FACE('',(#2155),#225,.T.);
#9143=ADVANCED_FACE('',(#2156),#382,.T.);
#9144=ADVANCED_FACE('',(#2157),#383,.T.);
#9145=ADVANCED_FACE('',(#2158),#226,.T.);
#9146=ADVANCED_FACE('',(#2159),#384,.T.);
#9147=ADVANCED_FACE('',(#2160),#385,.T.);
#9148=ADVANCED_FACE('',(#2161),#386,.F.);
#9149=ADVANCED_FACE('',(#2162),#387,.T.);
#9150=ADVANCED_FACE('',(#2163),#388,.T.);
#9151=ADVANCED_FACE('',(#2164),#389,.T.);
#9152=ADVANCED_FACE('',(#2165),#390,.T.);
#9153=ADVANCED_FACE('',(#2166),#391,.T.);
#9154=ADVANCED_FACE('',(#2167),#392,.T.);
#9155=ADVANCED_FACE('',(#2168),#393,.T.);
#9156=ADVANCED_FACE('',(#2169),#394,.T.);
#9157=ADVANCED_FACE('',(#2170),#395,.F.);
#9158=ADVANCED_FACE('',(#2171),#396,.T.);
#9159=ADVANCED_FACE('',(#2172),#397,.T.);
#9160=ADVANCED_FACE('',(#2173),#398,.T.);
#9161=ADVANCED_FACE('',(#2174),#399,.T.);
#9162=ADVANCED_FACE('',(#2175),#400,.T.);
#9163=ADVANCED_FACE('',(#2176),#401,.T.);
#9164=ADVANCED_FACE('',(#2177),#402,.T.);
#9165=ADVANCED_FACE('',(#2178),#403,.F.);
#9166=ADVANCED_FACE('',(#2179),#404,.T.);
#9167=ADVANCED_FACE('',(#2180),#405,.F.);
#9168=ADVANCED_FACE('',(#2181),#406,.T.);
#9169=ADVANCED_FACE('',(#2182),#407,.T.);
#9170=ADVANCED_FACE('',(#2183),#8892,.T.);
#9171=ADVANCED_FACE('',(#2184),#8893,.T.);
#9172=ADVANCED_FACE('',(#2185,#1975,#1976),#8894,.F.);
#9173=ADVANCED_FACE('',(#2186),#8895,.T.);
#9174=ADVANCED_FACE('',(#2187),#8896,.F.);
#9175=ADVANCED_FACE('',(#2188),#8897,.T.);
#9176=ADVANCED_FACE('',(#2189),#8898,.T.);
#9177=ADVANCED_FACE('',(#2190),#8899,.T.);
#9178=ADVANCED_FACE('',(#2191,#1977,#1978,#1979,#1980),#8900,.T.);
#9179=ADVANCED_FACE('',(#2192),#8901,.T.);
#9180=ADVANCED_FACE('',(#2193),#8902,.T.);
#9181=ADVANCED_FACE('',(#2194),#8903,.T.);
#9182=ADVANCED_FACE('',(#2195),#8904,.T.);
#9183=ADVANCED_FACE('',(#2196),#8905,.T.);
#9184=ADVANCED_FACE('',(#2197),#408,.F.);
#9185=ADVANCED_FACE('',(#2198),#8906,.F.);
#9186=ADVANCED_FACE('',(#2199),#409,.F.);
#9187=ADVANCED_FACE('',(#2200),#8907,.F.);
#9188=ADVANCED_FACE('',(#2201),#410,.F.);
#9189=ADVANCED_FACE('',(#2202),#8908,.F.);
#9190=ADVANCED_FACE('',(#2203),#411,.F.);
#9191=ADVANCED_FACE('',(#2204),#8909,.F.);
#9192=ADVANCED_FACE('',(#2205),#412,.F.);
#9193=ADVANCED_FACE('',(#2206),#8910,.T.);
#9194=ADVANCED_FACE('',(#2207),#413,.F.);
#9195=ADVANCED_FACE('',(#2208),#8911,.T.);
#9196=ADVANCED_FACE('',(#2209),#414,.F.);
#9197=ADVANCED_FACE('',(#2210),#8912,.T.);
#9198=ADVANCED_FACE('',(#2211),#415,.F.);
#9199=ADVANCED_FACE('',(#2212),#8913,.T.);
#9200=ADVANCED_FACE('',(#2213),#8914,.T.);
#9201=ADVANCED_FACE('',(#2214),#8915,.T.);
#9202=ADVANCED_FACE('',(#2215),#8916,.T.);
#9203=ADVANCED_FACE('',(#2216),#416,.T.);
#9204=ADVANCED_FACE('',(#2217),#417,.T.);
#9205=ADVANCED_FACE('',(#2218),#8917,.T.);
#9206=ADVANCED_FACE('',(#2219,#1981,#1982,#1983,#1984),#8918,.T.);
#9207=ADVANCED_FACE('',(#2220),#418,.T.);
#9208=ADVANCED_FACE('',(#2221),#419,.T.);
#9209=ADVANCED_FACE('',(#2222),#8919,.T.);
#9210=ADVANCED_FACE('',(#2223),#8920,.F.);
#9211=ADVANCED_FACE('',(#2224),#8921,.F.);
#9212=ADVANCED_FACE('',(#2225),#8922,.F.);
#9213=ADVANCED_FACE('',(#2226),#420,.T.);
#9214=ADVANCED_FACE('',(#2227),#8923,.T.);
#9215=ADVANCED_FACE('',(#2228,#1985,#1986,#1987,#1988),#8924,.T.);
#9216=ADVANCED_FACE('',(#2229),#421,.T.);
#9217=ADVANCED_FACE('',(#2230),#227,.T.);
#9218=ADVANCED_FACE('',(#2231),#228,.T.);
#9219=ADVANCED_FACE('',(#2232),#149,.T.);
#9220=ADVANCED_FACE('',(#2233),#150,.T.);
#9221=ADVANCED_FACE('',(#2234),#422,.T.);
#9222=ADVANCED_FACE('',(#2235),#151,.T.);
#9223=ADVANCED_FACE('',(#2236),#423,.T.);
#9224=ADVANCED_FACE('',(#2237),#424,.T.);
#9225=ADVANCED_FACE('',(#2238),#152,.T.);
#9226=ADVANCED_FACE('',(#2239),#425,.T.);
#9227=ADVANCED_FACE('',(#2240),#426,.T.);
#9228=ADVANCED_FACE('',(#2241),#229,.T.);
#9229=ADVANCED_FACE('',(#2242),#153,.T.);
#9230=ADVANCED_FACE('',(#2243),#230,.T.);
#9231=ADVANCED_FACE('',(#2244),#427,.T.);
#9232=ADVANCED_FACE('',(#2245),#428,.F.);
#9233=ADVANCED_FACE('',(#2246),#154,.T.);
#9234=ADVANCED_FACE('',(#2247),#231,.T.);
#9235=ADVANCED_FACE('',(#2248),#232,.T.);
#9236=ADVANCED_FACE('',(#2249),#429,.T.);
#9237=ADVANCED_FACE('',(#2250),#430,.F.);
#9238=ADVANCED_FACE('',(#2251),#155,.T.);
#9239=ADVANCED_FACE('',(#2252),#156,.T.);
#9240=ADVANCED_FACE('',(#2253),#431,.T.);
#9241=ADVANCED_FACE('',(#2254),#157,.T.);
#9242=ADVANCED_FACE('',(#2255),#432,.T.);
#9243=ADVANCED_FACE('',(#2256),#433,.T.);
#9244=ADVANCED_FACE('',(#2257),#158,.T.);
#9245=ADVANCED_FACE('',(#2258),#434,.T.);
#9246=ADVANCED_FACE('',(#2259),#435,.T.);
#9247=ADVANCED_FACE('',(#2260),#233,.T.);
#9248=ADVANCED_FACE('',(#2261),#159,.T.);
#9249=ADVANCED_FACE('',(#2262),#436,.T.);
#9250=ADVANCED_FACE('',(#2263),#234,.T.);
#9251=ADVANCED_FACE('',(#2264),#160,.T.);
#9252=ADVANCED_FACE('',(#2265),#437,.T.);
#9253=ADVANCED_FACE('',(#2266),#161,.T.);
#9254=ADVANCED_FACE('',(#2267),#438,.T.);
#9255=ADVANCED_FACE('',(#2268),#439,.T.);
#9256=ADVANCED_FACE('',(#2269),#162,.T.);
#9257=ADVANCED_FACE('',(#2270),#440,.T.);
#9258=ADVANCED_FACE('',(#2271),#441,.T.);
#9259=ADVANCED_FACE('',(#2272),#442,.T.);
#9260=ADVANCED_FACE('',(#2273),#443,.T.);
#9261=ADVANCED_FACE('',(#2274),#444,.T.);
#9262=ADVANCED_FACE('',(#2275),#445,.F.);
#9263=ADVANCED_FACE('',(#2276),#446,.T.);
#9264=ADVANCED_FACE('',(#2277),#447,.T.);
#9265=ADVANCED_FACE('',(#2278),#448,.T.);
#9266=ADVANCED_FACE('',(#2279),#449,.T.);
#9267=ADVANCED_FACE('',(#2280),#450,.T.);
#9268=ADVANCED_FACE('',(#2281),#451,.T.);
#9269=ADVANCED_FACE('',(#2282),#452,.T.);
#9270=ADVANCED_FACE('',(#2283),#453,.T.);
#9271=ADVANCED_FACE('',(#2284),#454,.F.);
#9272=ADVANCED_FACE('',(#2285),#8925,.F.);
#9273=ADVANCED_FACE('',(#2286),#8926,.F.);
#9274=ADVANCED_FACE('',(#2287),#8927,.F.);
#9275=ADVANCED_FACE('',(#2288),#8928,.F.);
#9276=ADVANCED_FACE('',(#2289),#8929,.F.);
#9277=ADVANCED_FACE('',(#2290),#8930,.F.);
#9278=ADVANCED_FACE('',(#2291),#8931,.F.);
#9279=ADVANCED_FACE('',(#2292),#8932,.T.);
#9280=ADVANCED_FACE('',(#2293),#8933,.F.);
#9281=ADVANCED_FACE('',(#2294),#8934,.T.);
#9282=ADVANCED_FACE('',(#2295),#8935,.T.);
#9283=ADVANCED_FACE('',(#2296),#455,.T.);
#9284=ADVANCED_FACE('',(#2297),#235,.T.);
#9285=ADVANCED_FACE('',(#2298),#456,.T.);
#9286=ADVANCED_FACE('',(#2299),#236,.T.);
#9287=ADVANCED_FACE('',(#2300),#457,.F.);
#9288=ADVANCED_FACE('',(#2301),#8936,.T.);
#9289=ADVANCED_FACE('',(#2302,#1989),#8937,.F.);
#9290=ADVANCED_FACE('',(#2303),#237,.T.);
#9291=ADVANCED_FACE('',(#2304),#163,.T.);
#9292=ADVANCED_FACE('',(#2305),#238,.T.);
#9293=ADVANCED_FACE('',(#2306),#458,.T.);
#9294=ADVANCED_FACE('',(#2307),#164,.T.);
#9295=ADVANCED_FACE('',(#2308),#165,.T.);
#9296=ADVANCED_FACE('',(#2309),#459,.T.);
#9297=ADVANCED_FACE('',(#2310),#166,.T.);
#9298=ADVANCED_FACE('',(#2311),#167,.T.);
#9299=ADVANCED_FACE('',(#2312),#168,.T.);
#9300=ADVANCED_FACE('',(#2313),#169,.T.);
#9301=ADVANCED_FACE('',(#2314),#460,.T.);
#9302=ADVANCED_FACE('',(#2315),#170,.T.);
#9303=ADVANCED_FACE('',(#2316),#461,.T.);
#9304=ADVANCED_FACE('',(#2317),#462,.T.);
#9305=ADVANCED_FACE('',(#2318),#463,.T.);
#9306=ADVANCED_FACE('',(#2319),#464,.T.);
#9307=ADVANCED_FACE('',(#2320),#465,.T.);
#9308=ADVANCED_FACE('',(#2321),#466,.T.);
#9309=ADVANCED_FACE('',(#2322),#467,.T.);
#9310=ADVANCED_FACE('',(#2323),#468,.T.);
#9311=ADVANCED_FACE('',(#2324),#469,.T.);
#9312=ADVANCED_FACE('',(#2325),#470,.T.);
#9313=ADVANCED_FACE('',(#2326),#471,.T.);
#9314=ADVANCED_FACE('',(#2327),#472,.F.);
#9315=ADVANCED_FACE('',(#2328),#473,.T.);
#9316=ADVANCED_FACE('',(#2329),#474,.T.);
#9317=ADVANCED_FACE('',(#2330),#8938,.F.);
#9318=ADVANCED_FACE('',(#2331),#8939,.T.);
#9319=ADVANCED_FACE('',(#2332),#8940,.F.);
#9320=ADVANCED_FACE('',(#2333,#1990),#8941,.F.);
#9321=ADVANCED_FACE('',(#2334),#8942,.F.);
#9322=ADVANCED_FACE('',(#2335),#8943,.F.);
#9323=ADVANCED_FACE('',(#2336),#475,.T.);
#9324=ADVANCED_FACE('',(#2337),#239,.T.);
#9325=ADVANCED_FACE('',(#2338),#476,.T.);
#9326=ADVANCED_FACE('',(#2339),#240,.T.);
#9327=ADVANCED_FACE('',(#2340),#477,.F.);
#9328=ADVANCED_FACE('',(#2341),#8944,.T.);
#9329=ADVANCED_FACE('',(#2342),#8945,.F.);
#9330=ADVANCED_FACE('',(#2343),#478,.F.);
#9331=ADVANCED_FACE('',(#2344),#479,.F.);
#9332=ADVANCED_FACE('',(#2345),#8946,.T.);
#9333=ADVANCED_FACE('',(#2346),#480,.T.);
#9334=ADVANCED_FACE('',(#2347),#8947,.T.);
#9335=ADVANCED_FACE('',(#2348),#481,.F.);
#9336=ADVANCED_FACE('',(#2349),#482,.F.);
#9337=ADVANCED_FACE('',(#2350),#483,.F.);
#9338=ADVANCED_FACE('',(#2351),#484,.F.);
#9339=ADVANCED_FACE('',(#2352),#485,.F.);
#9340=ADVANCED_FACE('',(#2353),#486,.F.);
#9341=ADVANCED_FACE('',(#2354),#487,.F.);
#9342=ADVANCED_FACE('',(#2355),#488,.F.);
#9343=ADVANCED_FACE('',(#2356),#489,.F.);
#9344=ADVANCED_FACE('',(#2357),#490,.F.);
#9345=ADVANCED_FACE('',(#2358),#491,.F.);
#9346=ADVANCED_FACE('',(#2359),#492,.F.);
#9347=ADVANCED_FACE('',(#2360),#493,.F.);
#9348=ADVANCED_FACE('',(#2361),#494,.F.);
#9349=ADVANCED_FACE('',(#2362),#495,.F.);
#9350=ADVANCED_FACE('',(#2363),#496,.F.);
#9351=ADVANCED_FACE('',(#2364),#497,.F.);
#9352=ADVANCED_FACE('',(#2365),#498,.F.);
#9353=ADVANCED_FACE('',(#2366),#499,.F.);
#9354=ADVANCED_FACE('',(#2367),#500,.F.);
#9355=ADVANCED_FACE('',(#2368),#501,.F.);
#9356=ADVANCED_FACE('',(#2369),#502,.F.);
#9357=ADVANCED_FACE('',(#2370),#503,.F.);
#9358=ADVANCED_FACE('',(#2371),#504,.F.);
#9359=ADVANCED_FACE('',(#2372),#505,.F.);
#9360=ADVANCED_FACE('',(#2373),#8948,.T.);
#9361=ADVANCED_FACE('',(#2374),#8949,.T.);
#9362=ADVANCED_FACE('',(#2375),#8950,.T.);
#9363=ADVANCED_FACE('',(#2376),#8951,.T.);
#9364=ADVANCED_FACE('',(#2377),#506,.T.);
#9365=ADVANCED_FACE('',(#2378),#507,.T.);
#9366=ADVANCED_FACE('',(#2379),#508,.T.);
#9367=ADVANCED_FACE('',(#2380),#509,.T.);
#9368=ADVANCED_FACE('',(#2381),#510,.T.);
#9369=ADVANCED_FACE('',(#2382),#511,.T.);
#9370=ADVANCED_FACE('',(#2383),#512,.T.);
#9371=ADVANCED_FACE('',(#2384),#513,.T.);
#9372=ADVANCED_FACE('',(#2385),#514,.T.);
#9373=ADVANCED_FACE('',(#2386),#8952,.T.);
#9374=ADVANCED_FACE('',(#2387),#8953,.T.);
#9375=ADVANCED_FACE('',(#2388),#8954,.T.);
#9376=ADVANCED_FACE('',(#2389),#8955,.T.);
#9377=ADVANCED_FACE('',(#2390),#8956,.T.);
#9378=ADVANCED_FACE('',(#2391),#515,.F.);
#9379=ADVANCED_FACE('',(#2392),#516,.F.);
#9380=ADVANCED_FACE('',(#2393),#517,.F.);
#9381=ADVANCED_FACE('',(#2394),#518,.F.);
#9382=ADVANCED_FACE('',(#2395),#519,.F.);
#9383=ADVANCED_FACE('',(#2396),#520,.F.);
#9384=ADVANCED_FACE('',(#2397),#521,.F.);
#9385=ADVANCED_FACE('',(#2398),#522,.F.);
#9386=ADVANCED_FACE('',(#2399),#523,.F.);
#9387=ADVANCED_FACE('',(#2400),#8957,.T.);
#9388=ADVANCED_FACE('',(#2401),#8958,.T.);
#9389=ADVANCED_FACE('',(#2402),#8959,.T.);
#9390=ADVANCED_FACE('',(#2403),#8960,.T.);
#9391=ADVANCED_FACE('',(#2404),#8961,.T.);
#9392=ADVANCED_FACE('',(#2405),#8962,.T.);
#9393=ADVANCED_FACE('',(#2406),#8963,.T.);
#9394=ADVANCED_FACE('',(#2407),#8964,.T.);
#9395=ADVANCED_FACE('',(#2408),#524,.T.);
#9396=ADVANCED_FACE('',(#2409),#525,.T.);
#9397=ADVANCED_FACE('',(#2410),#526,.T.);
#9398=ADVANCED_FACE('',(#2411),#527,.T.);
#9399=ADVANCED_FACE('',(#2412),#8965,.F.);
#9400=ADVANCED_FACE('',(#2413),#528,.F.);
#9401=ADVANCED_FACE('',(#2414),#529,.F.);
#9402=ADVANCED_FACE('',(#2415),#530,.F.);
#9403=ADVANCED_FACE('',(#2416),#531,.F.);
#9404=ADVANCED_FACE('',(#2417),#532,.F.);
#9405=ADVANCED_FACE('',(#2418),#8966,.T.);
#9406=ADVANCED_FACE('',(#2419),#8967,.T.);
#9407=ADVANCED_FACE('',(#2420),#8968,.T.);
#9408=ADVANCED_FACE('',(#2421),#8969,.T.);
#9409=ADVANCED_FACE('',(#2422),#533,.T.);
#9410=ADVANCED_FACE('',(#2423),#534,.T.);
#9411=ADVANCED_FACE('',(#2424),#535,.T.);
#9412=ADVANCED_FACE('',(#2425),#536,.T.);
#9413=ADVANCED_FACE('',(#2426,#1991,#1992,#1993),#8970,.T.);
#9414=ADVANCED_FACE('',(#2427,#1994,#1995,#1996,#1997,#1998),#8971,.F.);
#9415=ADVANCED_FACE('',(#2428),#171,.T.);
#9416=ADVANCED_FACE('',(#2429),#172,.T.);
#9417=ADVANCED_FACE('',(#2430),#241,.T.);
#9418=ADVANCED_FACE('',(#2431),#537,.T.);
#9419=ADVANCED_FACE('',(#2432),#242,.T.);
#9420=ADVANCED_FACE('',(#2433),#243,.T.);
#9421=ADVANCED_FACE('',(#2434),#244,.T.);
#9422=ADVANCED_FACE('',(#2435),#538,.T.);
#9423=ADVANCED_FACE('',(#2436),#173,.T.);
#9424=ADVANCED_FACE('',(#2437),#539,.T.);
#9425=ADVANCED_FACE('',(#2438),#174,.T.);
#9426=ADVANCED_FACE('',(#2439),#540,.T.);
#9427=ADVANCED_FACE('',(#2440),#175,.T.);
#9428=ADVANCED_FACE('',(#2441),#176,.T.);
#9429=ADVANCED_FACE('',(#2442),#541,.T.);
#9430=ADVANCED_FACE('',(#2443),#177,.T.);
#9431=ADVANCED_FACE('',(#2444),#542,.T.);
#9432=ADVANCED_FACE('',(#2445),#178,.T.);
#9433=ADVANCED_FACE('',(#2446),#543,.T.);
#9434=ADVANCED_FACE('',(#2447),#179,.T.);
#9435=ADVANCED_FACE('',(#2448),#180,.T.);
#9436=ADVANCED_FACE('',(#2449),#544,.T.);
#9437=ADVANCED_FACE('',(#2450),#245,.T.);
#9438=ADVANCED_FACE('',(#2451),#545,.T.);
#9439=ADVANCED_FACE('',(#2452),#181,.T.);
#9440=ADVANCED_FACE('',(#2453),#246,.T.);
#9441=ADVANCED_FACE('',(#2454),#182,.T.);
#9442=ADVANCED_FACE('',(#2455),#183,.T.);
#9443=ADVANCED_FACE('',(#2456),#546,.T.);
#9444=ADVANCED_FACE('',(#2457),#184,.T.);
#9445=ADVANCED_FACE('',(#2458),#185,.T.);
#9446=ADVANCED_FACE('',(#2459),#186,.T.);
#9447=ADVANCED_FACE('',(#2460),#247,.T.);
#9448=ADVANCED_FACE('',(#2461),#547,.T.);
#9449=ADVANCED_FACE('',(#2462),#548,.T.);
#9450=ADVANCED_FACE('',(#2463),#248,.T.);
#9451=ADVANCED_FACE('',(#2464),#549,.T.);
#9452=ADVANCED_FACE('',(#2465),#550,.T.);
#9453=ADVANCED_FACE('',(#2466),#551,.T.);
#9454=ADVANCED_FACE('',(#2467),#552,.T.);
#9455=ADVANCED_FACE('',(#2468),#553,.T.);
#9456=ADVANCED_FACE('',(#2469),#554,.T.);
#9457=ADVANCED_FACE('',(#2470),#555,.T.);
#9458=ADVANCED_FACE('',(#2471),#556,.T.);
#9459=ADVANCED_FACE('',(#2472),#557,.T.);
#9460=ADVANCED_FACE('',(#2473),#558,.T.);
#9461=ADVANCED_FACE('',(#2474),#559,.T.);
#9462=ADVANCED_FACE('',(#2475),#560,.T.);
#9463=ADVANCED_FACE('',(#2476),#561,.T.);
#9464=ADVANCED_FACE('',(#2477),#562,.T.);
#9465=ADVANCED_FACE('',(#2478),#563,.T.);
#9466=ADVANCED_FACE('',(#2479),#564,.T.);
#9467=ADVANCED_FACE('',(#2480),#565,.F.);
#9468=ADVANCED_FACE('',(#2481),#566,.T.);
#9469=ADVANCED_FACE('',(#2482),#567,.T.);
#9470=ADVANCED_FACE('',(#2483),#568,.T.);
#9471=ADVANCED_FACE('',(#2484),#8972,.T.);
#9472=ADVANCED_FACE('',(#2485),#8973,.T.);
#9473=ADVANCED_FACE('',(#2486),#8974,.T.);
#9474=ADVANCED_FACE('',(#2487),#8975,.T.);
#9475=ADVANCED_FACE('',(#2488),#8976,.T.);
#9476=ADVANCED_FACE('',(#2489,#1999,#2000,#2001,#2002,#2003,#2004,#2005,
#2006,#2007,#2008,#2009,#2010,#2011,#2012,#2013,#2014,#2015,#2016,#2017,
#2018,#2019),#8977,.T.);
#9477=ADVANCED_FACE('',(#2490),#8978,.T.);
#9478=ADVANCED_FACE('',(#2491),#8979,.T.);
#9479=ADVANCED_FACE('',(#2492),#8980,.T.);
#9480=ADVANCED_FACE('',(#2493),#569,.T.);
#9481=ADVANCED_FACE('',(#2494),#249,.T.);
#9482=ADVANCED_FACE('',(#2495),#570,.T.);
#9483=ADVANCED_FACE('',(#2496),#250,.T.);
#9484=ADVANCED_FACE('',(#2497),#571,.F.);
#9485=ADVANCED_FACE('',(#2498),#8981,.F.);
#9486=ADVANCED_FACE('',(#2499,#2020),#8982,.T.);
#9487=ADVANCED_FACE('',(#2500),#251,.T.);
#9488=ADVANCED_FACE('',(#2501),#187,.T.);
#9489=ADVANCED_FACE('',(#2502),#252,.T.);
#9490=ADVANCED_FACE('',(#2503),#572,.T.);
#9491=ADVANCED_FACE('',(#2504),#188,.T.);
#9492=ADVANCED_FACE('',(#2505),#189,.T.);
#9493=ADVANCED_FACE('',(#2506),#573,.T.);
#9494=ADVANCED_FACE('',(#2507),#190,.T.);
#9495=ADVANCED_FACE('',(#2508),#191,.T.);
#9496=ADVANCED_FACE('',(#2509),#192,.T.);
#9497=ADVANCED_FACE('',(#2510),#193,.T.);
#9498=ADVANCED_FACE('',(#2511),#574,.T.);
#9499=ADVANCED_FACE('',(#2512),#194,.T.);
#9500=ADVANCED_FACE('',(#2513),#575,.T.);
#9501=ADVANCED_FACE('',(#2514),#576,.T.);
#9502=ADVANCED_FACE('',(#2515),#577,.T.);
#9503=ADVANCED_FACE('',(#2516),#578,.T.);
#9504=ADVANCED_FACE('',(#2517),#579,.T.);
#9505=ADVANCED_FACE('',(#2518),#580,.T.);
#9506=ADVANCED_FACE('',(#2519),#581,.T.);
#9507=ADVANCED_FACE('',(#2520),#582,.T.);
#9508=ADVANCED_FACE('',(#2521),#583,.T.);
#9509=ADVANCED_FACE('',(#2522),#584,.T.);
#9510=ADVANCED_FACE('',(#2523),#585,.T.);
#9511=ADVANCED_FACE('',(#2524),#586,.F.);
#9512=ADVANCED_FACE('',(#2525),#587,.T.);
#9513=ADVANCED_FACE('',(#2526),#588,.T.);
#9514=ADVANCED_FACE('',(#2527),#8983,.T.);
#9515=ADVANCED_FACE('',(#2528),#8984,.F.);
#9516=ADVANCED_FACE('',(#2529),#8985,.T.);
#9517=ADVANCED_FACE('',(#2530,#2021),#8986,.T.);
#9518=ADVANCED_FACE('',(#2531),#8987,.T.);
#9519=ADVANCED_FACE('',(#2532),#8988,.T.);
#9520=ADVANCED_FACE('',(#2533),#589,.T.);
#9521=ADVANCED_FACE('',(#2534),#253,.T.);
#9522=ADVANCED_FACE('',(#2535),#590,.T.);
#9523=ADVANCED_FACE('',(#2536),#254,.T.);
#9524=ADVANCED_FACE('',(#2537),#591,.F.);
#9525=ADVANCED_FACE('',(#2538),#8989,.F.);
#9526=ADVANCED_FACE('',(#2539),#8990,.T.);
#9527=ADVANCED_FACE('',(#2540,#2022),#8991,.F.);
#9528=ADVANCED_FACE('',(#2541),#1972,.T.);
#9529=ADVANCED_FACE('',(#2542),#592,.T.);
#9530=ADVANCED_FACE('',(#2543),#8992,.T.);
#9531=ADVANCED_FACE('',(#2544),#1973,.T.);
#9532=ADVANCED_FACE('',(#2545),#593,.T.);
#9533=ADVANCED_FACE('',(#2546),#8993,.F.);
#9534=ADVANCED_FACE('',(#2547),#594,.T.);
#9535=ADVANCED_FACE('',(#2548),#255,.T.);
#9536=ADVANCED_FACE('',(#2549),#595,.T.);
#9537=ADVANCED_FACE('',(#2550),#256,.T.);
#9538=ADVANCED_FACE('',(#2551),#596,.F.);
#9539=ADVANCED_FACE('',(#2552),#8994,.T.);
#9540=ADVANCED_FACE('',(#2553,#2023),#8995,.F.);
#9541=ADVANCED_FACE('',(#2554),#257,.T.);
#9542=ADVANCED_FACE('',(#2555),#195,.T.);
#9543=ADVANCED_FACE('',(#2556),#258,.T.);
#9544=ADVANCED_FACE('',(#2557),#597,.T.);
#9545=ADVANCED_FACE('',(#2558),#196,.T.);
#9546=ADVANCED_FACE('',(#2559),#197,.T.);
#9547=ADVANCED_FACE('',(#2560),#598,.T.);
#9548=ADVANCED_FACE('',(#2561),#198,.T.);
#9549=ADVANCED_FACE('',(#2562),#199,.T.);
#9550=ADVANCED_FACE('',(#2563),#200,.T.);
#9551=ADVANCED_FACE('',(#2564),#201,.T.);
#9552=ADVANCED_FACE('',(#2565),#599,.T.);
#9553=ADVANCED_FACE('',(#2566),#202,.T.);
#9554=ADVANCED_FACE('',(#2567),#600,.T.);
#9555=ADVANCED_FACE('',(#2568),#601,.T.);
#9556=ADVANCED_FACE('',(#2569),#602,.T.);
#9557=ADVANCED_FACE('',(#2570),#603,.T.);
#9558=ADVANCED_FACE('',(#2571),#604,.T.);
#9559=ADVANCED_FACE('',(#2572),#605,.T.);
#9560=ADVANCED_FACE('',(#2573),#606,.T.);
#9561=ADVANCED_FACE('',(#2574),#607,.T.);
#9562=ADVANCED_FACE('',(#2575),#608,.T.);
#9563=ADVANCED_FACE('',(#2576),#609,.T.);
#9564=ADVANCED_FACE('',(#2577),#610,.T.);
#9565=ADVANCED_FACE('',(#2578),#611,.F.);
#9566=ADVANCED_FACE('',(#2579),#612,.T.);
#9567=ADVANCED_FACE('',(#2580),#613,.T.);
#9568=ADVANCED_FACE('',(#2581),#8996,.F.);
#9569=ADVANCED_FACE('',(#2582),#8997,.T.);
#9570=ADVANCED_FACE('',(#2583),#8998,.F.);
#9571=ADVANCED_FACE('',(#2584,#2024),#8999,.F.);
#9572=ADVANCED_FACE('',(#2585),#9000,.F.);
#9573=ADVANCED_FACE('',(#2586),#9001,.F.);
#9574=ADVANCED_FACE('',(#2587),#614,.T.);
#9575=ADVANCED_FACE('',(#2588),#259,.T.);
#9576=ADVANCED_FACE('',(#2589),#615,.T.);
#9577=ADVANCED_FACE('',(#2590),#260,.T.);
#9578=ADVANCED_FACE('',(#2591),#616,.F.);
#9579=ADVANCED_FACE('',(#2592),#9002,.T.);
#9580=ADVANCED_FACE('',(#2593),#9003,.F.);
#9581=ADVANCED_FACE('',(#2594),#617,.T.);
#9582=ADVANCED_FACE('',(#2595),#261,.T.);
#9583=ADVANCED_FACE('',(#2596),#618,.T.);
#9584=ADVANCED_FACE('',(#2597),#262,.T.);
#9585=ADVANCED_FACE('',(#2598),#619,.F.);
#9586=ADVANCED_FACE('',(#2599),#9004,.F.);
#9587=ADVANCED_FACE('',(#2600,#2025),#9005,.T.);
#9588=ADVANCED_FACE('',(#2601),#263,.T.);
#9589=ADVANCED_FACE('',(#2602),#203,.T.);
#9590=ADVANCED_FACE('',(#2603),#264,.T.);
#9591=ADVANCED_FACE('',(#2604),#620,.T.);
#9592=ADVANCED_FACE('',(#2605),#204,.T.);
#9593=ADVANCED_FACE('',(#2606),#205,.T.);
#9594=ADVANCED_FACE('',(#2607),#621,.T.);
#9595=ADVANCED_FACE('',(#2608),#206,.T.);
#9596=ADVANCED_FACE('',(#2609),#207,.T.);
#9597=ADVANCED_FACE('',(#2610),#208,.T.);
#9598=ADVANCED_FACE('',(#2611),#209,.T.);
#9599=ADVANCED_FACE('',(#2612),#622,.T.);
#9600=ADVANCED_FACE('',(#2613),#210,.T.);
#9601=ADVANCED_FACE('',(#2614),#623,.T.);
#9602=ADVANCED_FACE('',(#2615),#624,.T.);
#9603=ADVANCED_FACE('',(#2616),#625,.T.);
#9604=ADVANCED_FACE('',(#2617),#626,.T.);
#9605=ADVANCED_FACE('',(#2618),#627,.T.);
#9606=ADVANCED_FACE('',(#2619),#628,.T.);
#9607=ADVANCED_FACE('',(#2620),#629,.T.);
#9608=ADVANCED_FACE('',(#2621),#630,.T.);
#9609=ADVANCED_FACE('',(#2622),#631,.T.);
#9610=ADVANCED_FACE('',(#2623),#632,.T.);
#9611=ADVANCED_FACE('',(#2624),#633,.T.);
#9612=ADVANCED_FACE('',(#2625),#634,.F.);
#9613=ADVANCED_FACE('',(#2626),#635,.T.);
#9614=ADVANCED_FACE('',(#2627),#636,.T.);
#9615=ADVANCED_FACE('',(#2628),#9006,.T.);
#9616=ADVANCED_FACE('',(#2629),#9007,.F.);
#9617=ADVANCED_FACE('',(#2630),#9008,.T.);
#9618=ADVANCED_FACE('',(#2631,#2026),#9009,.T.);
#9619=ADVANCED_FACE('',(#2632),#9010,.T.);
#9620=ADVANCED_FACE('',(#2633),#9011,.T.);
#9621=ADVANCED_FACE('',(#2634),#637,.T.);
#9622=ADVANCED_FACE('',(#2635),#265,.T.);
#9623=ADVANCED_FACE('',(#2636),#638,.T.);
#9624=ADVANCED_FACE('',(#2637),#266,.T.);
#9625=ADVANCED_FACE('',(#2638),#639,.F.);
#9626=ADVANCED_FACE('',(#2639),#9012,.F.);
#9627=ADVANCED_FACE('',(#2640),#9013,.T.);
#9628=CLOSED_SHELL('',(#9014,#9015,#9016,#9017,#9018,#9019,#9020));
#9629=CLOSED_SHELL('',(#9021,#9022,#9023,#9024,#9025,#9026,#9027,#9028,
#9029,#9030,#9031,#9032,#9033,#9034,#9035,#9036,#9037,#9038,#9039,#9040,
#9041,#9042,#9043,#9044,#9045,#9046,#9047,#9048,#9049,#9050,#9051,#9052,
#9053,#9054,#9055,#9056,#9057,#9058,#9059,#9060,#9061,#9062,#9063,#9064,
#9065,#9066,#9067,#9068,#9069,#9070,#9071,#9072,#9073,#9074,#9075,#9076,
#9077,#9078,#9079,#9080,#9081,#9082,#9083,#9084,#9085,#9086,#9087,#9088,
#9089,#9090,#9091,#9092,#9093,#9094,#9095,#9096,#9097,#9098,#9099,#9100,
#9101,#9102,#9103));
#9630=CLOSED_SHELL('',(#9104,#9105,#9106,#9107,#9108,#9109,#9110,#9111,
#9112,#9113,#9114,#9115,#9116,#9117,#9118,#9119,#9120,#9121,#9122,#9123,
#9124,#9125,#9126,#9127,#9128,#9129,#9130,#9131,#9132,#9133,#9134,#9135,
#9136,#9137,#9138,#9139,#9140,#9141,#9142,#9143,#9144,#9145,#9146,#9147,
#9148,#9149,#9150,#9151,#9152,#9153,#9154,#9155,#9156,#9157,#9158,#9159,
#9160,#9161,#9162,#9163,#9164,#9165,#9166,#9167,#9168,#9169,#9170,#9171,
#9172,#9173,#9174,#9175,#9176,#9177,#9178,#9179,#9180,#9181,#9182,#9183));
#9631=CLOSED_SHELL('',(#9184,#9185,#9186,#9187,#9188,#9189,#9190,#9191,
#9192,#9193,#9194,#9195,#9196,#9197,#9198,#9199,#9200,#9201,#9202,#9203,
#9204,#9205,#9206,#9207,#9208,#9209,#9210,#9211,#9212,#9213,#9214,#9215,
#9216,#9217,#9218,#9219,#9220,#9221,#9222,#9223,#9224,#9225,#9226,#9227,
#9228,#9229,#9230,#9231,#9232,#9233,#9234,#9235,#9236,#9237,#9238,#9239,
#9240,#9241,#9242,#9243,#9244,#9245,#9246,#9247,#9248,#9249,#9250,#9251,
#9252,#9253,#9254,#9255,#9256,#9257,#9258,#9259,#9260,#9261,#9262,#9263,
#9264,#9265,#9266,#9267,#9268,#9269,#9270,#9271,#9272,#9273,#9274,#9275,
#9276,#9277,#9278,#9279,#9280,#9281,#9282));
#9632=CLOSED_SHELL('',(#9283,#9284,#9285,#9286,#9287,#9288,#9289,#9290,
#9291,#9292,#9293,#9294,#9295,#9296,#9297,#9298,#9299,#9300,#9301,#9302,
#9303,#9304,#9305,#9306,#9307,#9308,#9309,#9310,#9311,#9312,#9313,#9314,
#9315,#9316,#9317,#9318,#9319,#9320,#9321,#9322,#9323,#9324,#9325,#9326,
#9327,#9328,#9329));
#9633=CLOSED_SHELL('',(#9330,#9331,#9332,#9333,#9334,#9335,#9336,#9337,
#9338,#9339,#9340,#9341,#9342,#9343,#9344,#9345,#9346,#9347,#9348,#9349,
#9350,#9351,#9352,#9353,#9354,#9355,#9356,#9357,#9358,#9359,#9360,#9361,
#9362,#9363,#9364,#9365,#9366,#9367,#9368,#9369,#9370,#9371,#9372,#9373,
#9374,#9375,#9376,#9377,#9378,#9379,#9380,#9381,#9382,#9383,#9384,#9385,
#9386,#9387,#9388,#9389,#9390,#9391,#9392,#9393,#9394,#9395,#9396,#9397,
#9398,#9399,#9400,#9401,#9402,#9403,#9404,#9405,#9406,#9407,#9408,#9409,
#9410,#9411,#9412,#9413,#9414,#9415,#9416,#9417,#9418,#9419,#9420,#9421,
#9422,#9423,#9424,#9425,#9426,#9427,#9428,#9429,#9430,#9431,#9432,#9433,
#9434,#9435,#9436,#9437,#9438,#9439,#9440,#9441,#9442,#9443,#9444,#9445,
#9446,#9447,#9448,#9449,#9450,#9451,#9452,#9453,#9454,#9455,#9456,#9457,
#9458,#9459,#9460,#9461,#9462,#9463,#9464,#9465,#9466,#9467,#9468,#9469,
#9470,#9471,#9472,#9473,#9474,#9475,#9476,#9477,#9478,#9479));
#9634=CLOSED_SHELL('',(#9480,#9481,#9482,#9483,#9484,#9485,#9486,#9487,
#9488,#9489,#9490,#9491,#9492,#9493,#9494,#9495,#9496,#9497,#9498,#9499,
#9500,#9501,#9502,#9503,#9504,#9505,#9506,#9507,#9508,#9509,#9510,#9511,
#9512,#9513,#9514,#9515,#9516,#9517,#9518,#9519,#9520,#9521,#9522,#9523,
#9524,#9525,#9526));
#9635=CLOSED_SHELL('',(#9527,#9528,#9529,#9530,#9531,#9532,#9533));
#9636=CLOSED_SHELL('',(#9534,#9535,#9536,#9537,#9538,#9539,#9540,#9541,
#9542,#9543,#9544,#9545,#9546,#9547,#9548,#9549,#9550,#9551,#9552,#9553,
#9554,#9555,#9556,#9557,#9558,#9559,#9560,#9561,#9562,#9563,#9564,#9565,
#9566,#9567,#9568,#9569,#9570,#9571,#9572,#9573,#9574,#9575,#9576,#9577,
#9578,#9579,#9580));
#9637=CLOSED_SHELL('',(#9581,#9582,#9583,#9584,#9585,#9586,#9587,#9588,
#9589,#9590,#9591,#9592,#9593,#9594,#9595,#9596,#9597,#9598,#9599,#9600,
#9601,#9602,#9603,#9604,#9605,#9606,#9607,#9608,#9609,#9610,#9611,#9612,
#9613,#9614,#9615,#9616,#9617,#9618,#9619,#9620,#9621,#9622,#9623,#9624,
#9625,#9626,#9627));
#9638=DERIVED_UNIT_ELEMENT(#9658,1.);
#9639=DERIVED_UNIT_ELEMENT(#17838,-3.);
#9640=DERIVED_UNIT_ELEMENT(#9658,1.);
#9641=DERIVED_UNIT_ELEMENT(#17838,-3.);
#9642=DERIVED_UNIT_ELEMENT(#9658,1.);
#9643=DERIVED_UNIT_ELEMENT(#17838,-3.);
#9644=DERIVED_UNIT_ELEMENT(#9658,1.);
#9645=DERIVED_UNIT_ELEMENT(#17838,-3.);
#9646=DERIVED_UNIT_ELEMENT(#9658,1.);
#9647=DERIVED_UNIT_ELEMENT(#17838,-3.);
#9648=DERIVED_UNIT_ELEMENT(#9658,1.);
#9649=DERIVED_UNIT_ELEMENT(#17838,-3.);
#9650=DERIVED_UNIT_ELEMENT(#9658,1.);
#9651=DERIVED_UNIT_ELEMENT(#17838,-3.);
#9652=DERIVED_UNIT_ELEMENT(#9658,1.);
#9653=DERIVED_UNIT_ELEMENT(#17838,-3.);
#9654=DERIVED_UNIT_ELEMENT(#9658,1.);
#9655=DERIVED_UNIT_ELEMENT(#17838,-3.);
#9656=DERIVED_UNIT_ELEMENT(#9658,1.);
#9657=DERIVED_UNIT_ELEMENT(#17838,-3.);
#9658=(
MASS_UNIT()
NAMED_UNIT(*)
SI_UNIT(.KILO.,.GRAM.)
);
#9659=DERIVED_UNIT((#9638,#9639));
#9660=DERIVED_UNIT((#9640,#9641));
#9661=DERIVED_UNIT((#9642,#9643));
#9662=DERIVED_UNIT((#9644,#9645));
#9663=DERIVED_UNIT((#9646,#9647));
#9664=DERIVED_UNIT((#9648,#9649));
#9665=DERIVED_UNIT((#9650,#9651));
#9666=DERIVED_UNIT((#9652,#9653));
#9667=DERIVED_UNIT((#9654,#9655));
#9668=DERIVED_UNIT((#9656,#9657));
#9669=MEASURE_REPRESENTATION_ITEM('density measure',
POSITIVE_RATIO_MEASURE(7850.),#9659);
#9670=MEASURE_REPRESENTATION_ITEM('density measure',
POSITIVE_RATIO_MEASURE(7850.),#9660);
#9671=MEASURE_REPRESENTATION_ITEM('density measure',
POSITIVE_RATIO_MEASURE(7850.),#9661);
#9672=MEASURE_REPRESENTATION_ITEM('density measure',
POSITIVE_RATIO_MEASURE(7850.),#9662);
#9673=MEASURE_REPRESENTATION_ITEM('density measure',
POSITIVE_RATIO_MEASURE(7850.),#9663);
#9674=MEASURE_REPRESENTATION_ITEM('density measure',
POSITIVE_RATIO_MEASURE(7850.),#9664);
#9675=MEASURE_REPRESENTATION_ITEM('density measure',
POSITIVE_RATIO_MEASURE(7850.),#9665);
#9676=MEASURE_REPRESENTATION_ITEM('density measure',
POSITIVE_RATIO_MEASURE(7850.),#9666);
#9677=MEASURE_REPRESENTATION_ITEM('density measure',
POSITIVE_RATIO_MEASURE(7850.),#9667);
#9678=MEASURE_REPRESENTATION_ITEM('density measure',
POSITIVE_RATIO_MEASURE(7850.),#9668);
#9679=PROPERTY_DEFINITION_REPRESENTATION(#9729,#9699);
#9680=PROPERTY_DEFINITION_REPRESENTATION(#9730,#9700);
#9681=PROPERTY_DEFINITION_REPRESENTATION(#9731,#9701);
#9682=PROPERTY_DEFINITION_REPRESENTATION(#9732,#9702);
#9683=PROPERTY_DEFINITION_REPRESENTATION(#9733,#9703);
#9684=PROPERTY_DEFINITION_REPRESENTATION(#9734,#9704);
#9685=PROPERTY_DEFINITION_REPRESENTATION(#9735,#9705);
#9686=PROPERTY_DEFINITION_REPRESENTATION(#9736,#9706);
#9687=PROPERTY_DEFINITION_REPRESENTATION(#9737,#9707);
#9688=PROPERTY_DEFINITION_REPRESENTATION(#9738,#9708);
#9689=PROPERTY_DEFINITION_REPRESENTATION(#9739,#9709);
#9690=PROPERTY_DEFINITION_REPRESENTATION(#9740,#9710);
#9691=PROPERTY_DEFINITION_REPRESENTATION(#9741,#9711);
#9692=PROPERTY_DEFINITION_REPRESENTATION(#9742,#9712);
#9693=PROPERTY_DEFINITION_REPRESENTATION(#9743,#9713);
#9694=PROPERTY_DEFINITION_REPRESENTATION(#9744,#9714);
#9695=PROPERTY_DEFINITION_REPRESENTATION(#9745,#9715);
#9696=PROPERTY_DEFINITION_REPRESENTATION(#9746,#9716);
#9697=PROPERTY_DEFINITION_REPRESENTATION(#9747,#9717);
#9698=PROPERTY_DEFINITION_REPRESENTATION(#9748,#9718);
#9699=REPRESENTATION('material name',(#9719),#17826);
#9700=REPRESENTATION('density',(#9669),#17826);
#9701=REPRESENTATION('material name',(#9720),#17827);
#9702=REPRESENTATION('density',(#9670),#17827);
#9703=REPRESENTATION('material name',(#9721),#17828);
#9704=REPRESENTATION('density',(#9671),#17828);
#9705=REPRESENTATION('material name',(#9722),#17829);
#9706=REPRESENTATION('density',(#9672),#17829);
#9707=REPRESENTATION('material name',(#9723),#17830);
#9708=REPRESENTATION('density',(#9673),#17830);
#9709=REPRESENTATION('material name',(#9724),#17831);
#9710=REPRESENTATION('density',(#9674),#17831);
#9711=REPRESENTATION('material name',(#9725),#17832);
#9712=REPRESENTATION('density',(#9675),#17832);
#9713=REPRESENTATION('material name',(#9726),#17833);
#9714=REPRESENTATION('density',(#9676),#17833);
#9715=REPRESENTATION('material name',(#9727),#17834);
#9716=REPRESENTATION('density',(#9677),#17834);
#9717=REPRESENTATION('material name',(#9728),#17835);
#9718=REPRESENTATION('density',(#9678),#17835);
#9719=DESCRIPTIVE_REPRESENTATION_ITEM('Steel','Steel');
#9720=DESCRIPTIVE_REPRESENTATION_ITEM('Steel','Steel');
#9721=DESCRIPTIVE_REPRESENTATION_ITEM('Steel','Steel');
#9722=DESCRIPTIVE_REPRESENTATION_ITEM('Steel','Steel');
#9723=DESCRIPTIVE_REPRESENTATION_ITEM('Steel','Steel');
#9724=DESCRIPTIVE_REPRESENTATION_ITEM('Steel','Steel');
#9725=DESCRIPTIVE_REPRESENTATION_ITEM('Steel','Steel');
#9726=DESCRIPTIVE_REPRESENTATION_ITEM('Steel','Steel');
#9727=DESCRIPTIVE_REPRESENTATION_ITEM('Steel','Steel');
#9728=DESCRIPTIVE_REPRESENTATION_ITEM('Steel','Steel');
#9729=PROPERTY_DEFINITION('material property','material name',#17886);
#9730=PROPERTY_DEFINITION('material property','density of part',#17886);
#9731=PROPERTY_DEFINITION('material property','material name',#17887);
#9732=PROPERTY_DEFINITION('material property','density of part',#17887);
#9733=PROPERTY_DEFINITION('material property','material name',#17888);
#9734=PROPERTY_DEFINITION('material property','density of part',#17888);
#9735=PROPERTY_DEFINITION('material property','material name',#17889);
#9736=PROPERTY_DEFINITION('material property','density of part',#17889);
#9737=PROPERTY_DEFINITION('material property','material name',#17890);
#9738=PROPERTY_DEFINITION('material property','density of part',#17890);
#9739=PROPERTY_DEFINITION('material property','material name',#17891);
#9740=PROPERTY_DEFINITION('material property','density of part',#17891);
#9741=PROPERTY_DEFINITION('material property','material name',#17892);
#9742=PROPERTY_DEFINITION('material property','density of part',#17892);
#9743=PROPERTY_DEFINITION('material property','material name',#17893);
#9744=PROPERTY_DEFINITION('material property','density of part',#17893);
#9745=PROPERTY_DEFINITION('material property','material name',#17894);
#9746=PROPERTY_DEFINITION('material property','density of part',#17894);
#9747=PROPERTY_DEFINITION('material property','material name',#17895);
#9748=PROPERTY_DEFINITION('material property','density of part',#17895);
#9749=AXIS2_PLACEMENT_3D('',#14263,#11032,#11033);
#9750=AXIS2_PLACEMENT_3D('',#14264,#11034,#11035);
#9751=AXIS2_PLACEMENT_3D('',#14265,#11036,#11037);
#9752=AXIS2_PLACEMENT_3D('',#14267,#11038,#11039);
#9753=AXIS2_PLACEMENT_3D('',#14269,#11040,#11041);
#9754=AXIS2_PLACEMENT_3D('',#14270,#11042,#11043);
#9755=AXIS2_PLACEMENT_3D('',#14272,#11044,#11045);
#9756=AXIS2_PLACEMENT_3D('',#14275,#11047,#11048);
#9757=AXIS2_PLACEMENT_3D('',#14276,#11049,#11050);
#9758=AXIS2_PLACEMENT_3D('',#14279,#11052,#11053);
#9759=AXIS2_PLACEMENT_3D('',#14280,#11054,#11055);
#9760=AXIS2_PLACEMENT_3D('',#14281,#11056,#11057);
#9761=AXIS2_PLACEMENT_3D('',#14283,#11059,#11060);
#9762=AXIS2_PLACEMENT_3D('',#14286,#11062,#11063);
#9763=AXIS2_PLACEMENT_3D('',#14287,#11064,#11065);
#9764=AXIS2_PLACEMENT_3D('',#14288,#11066,#11067);
#9765=AXIS2_PLACEMENT_3D('',#14289,#11068,#11069);
#9766=AXIS2_PLACEMENT_3D('',#14292,#11070,#11071);
#9767=AXIS2_PLACEMENT_3D('',#14300,#11075,#11076);
#9768=AXIS2_PLACEMENT_3D('',#14302,#11078,#11079);
#9769=AXIS2_PLACEMENT_3D('',#14305,#11080,#11081);
#9770=AXIS2_PLACEMENT_3D('',#14309,#11083,#11084);
#9771=AXIS2_PLACEMENT_3D('',#14315,#11088,#11089);
#9772=AXIS2_PLACEMENT_3D('',#14318,#11092,#11093);
#9773=AXIS2_PLACEMENT_3D('',#14322,#11095,#11096);
#9774=AXIS2_PLACEMENT_3D('',#14324,#11098,#11099);
#9775=AXIS2_PLACEMENT_3D('',#14328,#11101,#11102);
#9776=AXIS2_PLACEMENT_3D('',#14330,#11104,#11105);
#9777=AXIS2_PLACEMENT_3D('',#14334,#11108,#11109);
#9778=AXIS2_PLACEMENT_3D('',#14338,#11112,#11113);
#9779=AXIS2_PLACEMENT_3D('',#14340,#11114,#11115);
#9780=AXIS2_PLACEMENT_3D('',#14342,#11117,#11118);
#9781=AXIS2_PLACEMENT_3D('',#14345,#11120,#11121);
#9782=AXIS2_PLACEMENT_3D('',#14346,#11122,#11123);
#9783=AXIS2_PLACEMENT_3D('',#14364,#11132,#11133);
#9784=AXIS2_PLACEMENT_3D('',#14370,#11136,#11137);
#9785=AXIS2_PLACEMENT_3D('',#14374,#11139,#11140);
#9786=AXIS2_PLACEMENT_3D('',#14380,#11143,#11144);
#9787=AXIS2_PLACEMENT_3D('',#14384,#11147,#11148);
#9788=AXIS2_PLACEMENT_3D('',#14386,#11149,#11150);
#9789=AXIS2_PLACEMENT_3D('',#14392,#11153,#11154);
#9790=AXIS2_PLACEMENT_3D('',#14394,#11156,#11157);
#9791=AXIS2_PLACEMENT_3D('',#14396,#11158,#11159);
#9792=AXIS2_PLACEMENT_3D('',#14400,#11161,#11162);
#9793=AXIS2_PLACEMENT_3D('',#14404,#11165,#11166);
#9794=AXIS2_PLACEMENT_3D('',#14406,#11168,#11169);
#9795=AXIS2_PLACEMENT_3D('',#14409,#11171,#11172);
#9796=AXIS2_PLACEMENT_3D('',#14410,#11173,#11174);
#9797=AXIS2_PLACEMENT_3D('',#14416,#11177,#11178);
#9798=AXIS2_PLACEMENT_3D('',#14422,#11181,#11182);
#9799=AXIS2_PLACEMENT_3D('',#14426,#11184,#11185);
#9800=AXIS2_PLACEMENT_3D('',#14432,#11188,#11189);
#9801=AXIS2_PLACEMENT_3D('',#14441,#11195,#11196);
#9802=AXIS2_PLACEMENT_3D('',#14445,#11199,#11200);
#9803=AXIS2_PLACEMENT_3D('',#14448,#11202,#11203);
#9804=AXIS2_PLACEMENT_3D('',#14449,#11204,#11205);
#9805=AXIS2_PLACEMENT_3D('',#14451,#11206,#11207);
#9806=AXIS2_PLACEMENT_3D('',#14453,#11208,#11209);
#9807=AXIS2_PLACEMENT_3D('',#14454,#11210,#11211);
#9808=AXIS2_PLACEMENT_3D('',#14455,#11212,#11213);
#9809=AXIS2_PLACEMENT_3D('',#14457,#11214,#11215);
#9810=AXIS2_PLACEMENT_3D('',#14459,#11216,#11217);
#9811=AXIS2_PLACEMENT_3D('',#14460,#11218,#11219);
#9812=AXIS2_PLACEMENT_3D('',#14461,#11220,#11221);
#9813=AXIS2_PLACEMENT_3D('',#14463,#11222,#11223);
#9814=AXIS2_PLACEMENT_3D('',#14465,#11224,#11225);
#9815=AXIS2_PLACEMENT_3D('',#14466,#11226,#11227);
#9816=AXIS2_PLACEMENT_3D('',#14467,#11228,#11229);
#9817=AXIS2_PLACEMENT_3D('',#14469,#11230,#11231);
#9818=AXIS2_PLACEMENT_3D('',#14471,#11232,#11233);
#9819=AXIS2_PLACEMENT_3D('',#14472,#11234,#11235);
#9820=AXIS2_PLACEMENT_3D('',#14473,#11236,#11237);
#9821=AXIS2_PLACEMENT_3D('',#14475,#11239,#11240);
#9822=AXIS2_PLACEMENT_3D('',#14477,#11241,#11242);
#9823=AXIS2_PLACEMENT_3D('',#14479,#11243,#11244);
#9824=AXIS2_PLACEMENT_3D('',#14480,#11245,#11246);
#9825=AXIS2_PLACEMENT_3D('',#14481,#11247,#11248);
#9826=AXIS2_PLACEMENT_3D('',#14483,#11250,#11251);
#9827=AXIS2_PLACEMENT_3D('',#14486,#11254,#11255);
#9828=AXIS2_PLACEMENT_3D('',#14488,#11256,#11257);
#9829=AXIS2_PLACEMENT_3D('',#14490,#11258,#11259);
#9830=AXIS2_PLACEMENT_3D('',#14491,#11260,#11261);
#9831=AXIS2_PLACEMENT_3D('',#14492,#11262,#11263);
#9832=AXIS2_PLACEMENT_3D('',#14495,#11266,#11267);
#9833=AXIS2_PLACEMENT_3D('',#14497,#11269,#11270);
#9834=AXIS2_PLACEMENT_3D('',#14499,#11271,#11272);
#9835=AXIS2_PLACEMENT_3D('',#14501,#11273,#11274);
#9836=AXIS2_PLACEMENT_3D('',#14502,#11275,#11276);
#9837=AXIS2_PLACEMENT_3D('',#14503,#11277,#11278);
#9838=AXIS2_PLACEMENT_3D('',#14505,#11279,#11280);
#9839=AXIS2_PLACEMENT_3D('',#14506,#11281,#11282);
#9840=AXIS2_PLACEMENT_3D('',#14507,#11283,#11284);
#9841=AXIS2_PLACEMENT_3D('',#14509,#11285,#11286);
#9842=AXIS2_PLACEMENT_3D('',#14511,#11287,#11288);
#9843=AXIS2_PLACEMENT_3D('',#14512,#11289,#11290);
#9844=AXIS2_PLACEMENT_3D('',#14513,#11291,#11292);
#9845=AXIS2_PLACEMENT_3D('',#14515,#11294,#11295);
#9846=AXIS2_PLACEMENT_3D('',#14518,#11298,#11299);
#9847=AXIS2_PLACEMENT_3D('',#14520,#11300,#11301);
#9848=AXIS2_PLACEMENT_3D('',#14521,#11302,#11303);
#9849=AXIS2_PLACEMENT_3D('',#14522,#11304,#11305);
#9850=AXIS2_PLACEMENT_3D('',#14524,#11306,#11307);
#9851=AXIS2_PLACEMENT_3D('',#14526,#11308,#11309);
#9852=AXIS2_PLACEMENT_3D('',#14527,#11310,#11311);
#9853=AXIS2_PLACEMENT_3D('',#14528,#11312,#11313);
#9854=AXIS2_PLACEMENT_3D('',#14530,#11314,#11315);
#9855=AXIS2_PLACEMENT_3D('',#14532,#11316,#11317);
#9856=AXIS2_PLACEMENT_3D('',#14533,#11318,#11319);
#9857=AXIS2_PLACEMENT_3D('',#14534,#11320,#11321);
#9858=AXIS2_PLACEMENT_3D('',#14536,#11323,#11324);
#9859=AXIS2_PLACEMENT_3D('',#14539,#11327,#11328);
#9860=AXIS2_PLACEMENT_3D('',#14541,#11329,#11330);
#9861=AXIS2_PLACEMENT_3D('',#14543,#11331,#11332);
#9862=AXIS2_PLACEMENT_3D('',#14544,#11333,#11334);
#9863=AXIS2_PLACEMENT_3D('',#14545,#11335,#11336);
#9864=AXIS2_PLACEMENT_3D('',#14547,#11337,#11338);
#9865=AXIS2_PLACEMENT_3D('',#14549,#11339,#11340);
#9866=AXIS2_PLACEMENT_3D('',#14550,#11341,#11342);
#9867=AXIS2_PLACEMENT_3D('',#14551,#11343,#11344);
#9868=AXIS2_PLACEMENT_3D('',#14553,#11346,#11347);
#9869=AXIS2_PLACEMENT_3D('',#14555,#11348,#11349);
#9870=AXIS2_PLACEMENT_3D('',#14557,#11350,#11351);
#9871=AXIS2_PLACEMENT_3D('',#14558,#11352,#11353);
#9872=AXIS2_PLACEMENT_3D('',#14559,#11354,#11355);
#9873=AXIS2_PLACEMENT_3D('',#14561,#11357,#11358);
#9874=AXIS2_PLACEMENT_3D('',#14564,#11361,#11362);
#9875=AXIS2_PLACEMENT_3D('',#14566,#11363,#11364);
#9876=AXIS2_PLACEMENT_3D('',#14567,#11365,#11366);
#9877=AXIS2_PLACEMENT_3D('',#14568,#11367,#11368);
#9878=AXIS2_PLACEMENT_3D('',#14571,#11371,#11372);
#9879=AXIS2_PLACEMENT_3D('',#14573,#11374,#11375);
#9880=AXIS2_PLACEMENT_3D('',#14575,#11376,#11377);
#9881=AXIS2_PLACEMENT_3D('',#14577,#11378,#11379);
#9882=AXIS2_PLACEMENT_3D('',#14578,#11380,#11381);
#9883=AXIS2_PLACEMENT_3D('',#14579,#11382,#11383);
#9884=AXIS2_PLACEMENT_3D('',#14581,#11384,#11385);
#9885=AXIS2_PLACEMENT_3D('',#14582,#11386,#11387);
#9886=AXIS2_PLACEMENT_3D('',#14583,#11388,#11389);
#9887=AXIS2_PLACEMENT_3D('',#14585,#11391,#11392);
#9888=AXIS2_PLACEMENT_3D('',#14587,#11393,#11394);
#9889=AXIS2_PLACEMENT_3D('',#14589,#11395,#11396);
#9890=AXIS2_PLACEMENT_3D('',#14590,#11397,#11398);
#9891=AXIS2_PLACEMENT_3D('',#14591,#11399,#11400);
#9892=AXIS2_PLACEMENT_3D('',#14593,#11401,#11402);
#9893=AXIS2_PLACEMENT_3D('',#14594,#11403,#11404);
#9894=AXIS2_PLACEMENT_3D('',#14595,#11405,#11406);
#9895=AXIS2_PLACEMENT_3D('',#14596,#11407,#11408);
#9896=AXIS2_PLACEMENT_3D('',#14597,#11409,#11410);
#9897=AXIS2_PLACEMENT_3D('',#14600,#11411,#11412);
#9898=AXIS2_PLACEMENT_3D('',#14601,#11413,#11414);
#9899=AXIS2_PLACEMENT_3D('',#14602,#11415,#11416);
#9900=AXIS2_PLACEMENT_3D('',#14603,#11417,#11418);
#9901=AXIS2_PLACEMENT_3D('',#14605,#11420,#11421);
#9902=AXIS2_PLACEMENT_3D('',#14607,#11423,#11424);
#9903=AXIS2_PLACEMENT_3D('',#14609,#11425,#11426);
#9904=AXIS2_PLACEMENT_3D('',#14611,#11427,#11428);
#9905=AXIS2_PLACEMENT_3D('',#14612,#11429,#11430);
#9906=AXIS2_PLACEMENT_3D('',#14613,#11431,#11432);
#9907=AXIS2_PLACEMENT_3D('',#14616,#11435,#11436);
#9908=AXIS2_PLACEMENT_3D('',#14618,#11438,#11439);
#9909=AXIS2_PLACEMENT_3D('',#14620,#11441,#11442);
#9910=AXIS2_PLACEMENT_3D('',#14622,#11444,#11445);
#9911=AXIS2_PLACEMENT_3D('',#14624,#11447,#11448);
#9912=AXIS2_PLACEMENT_3D('',#14627,#11451,#11452);
#9913=AXIS2_PLACEMENT_3D('',#14629,#11454,#11455);
#9914=AXIS2_PLACEMENT_3D('',#14631,#11457,#11458);
#9915=AXIS2_PLACEMENT_3D('',#14633,#11460,#11461);
#9916=AXIS2_PLACEMENT_3D('',#14635,#11463,#11464);
#9917=AXIS2_PLACEMENT_3D('',#14637,#11466,#11467);
#9918=AXIS2_PLACEMENT_3D('',#14639,#11469,#11470);
#9919=AXIS2_PLACEMENT_3D('',#14641,#11472,#11473);
#9920=AXIS2_PLACEMENT_3D('',#14643,#11475,#11476);
#9921=AXIS2_PLACEMENT_3D('',#14646,#11479,#11480);
#9922=AXIS2_PLACEMENT_3D('',#14647,#11481,#11482);
#9923=AXIS2_PLACEMENT_3D('',#14648,#11483,#11484);
#9924=AXIS2_PLACEMENT_3D('',#14649,#11485,#11486);
#9925=AXIS2_PLACEMENT_3D('',#14650,#11487,#11488);
#9926=AXIS2_PLACEMENT_3D('',#14651,#11489,#11490);
#9927=AXIS2_PLACEMENT_3D('',#14652,#11491,#11492);
#9928=AXIS2_PLACEMENT_3D('',#14653,#11493,#11494);
#9929=AXIS2_PLACEMENT_3D('',#14654,#11495,#11496);
#9930=AXIS2_PLACEMENT_3D('',#14655,#11497,#11498);
#9931=AXIS2_PLACEMENT_3D('',#14656,#11499,#11500);
#9932=AXIS2_PLACEMENT_3D('',#14657,#11501,#11502);
#9933=AXIS2_PLACEMENT_3D('',#14658,#11503,#11504);
#9934=AXIS2_PLACEMENT_3D('',#14660,#11505,#11506);
#9935=AXIS2_PLACEMENT_3D('',#14663,#11508,#11509);
#9936=AXIS2_PLACEMENT_3D('',#14664,#11510,#11511);
#9937=AXIS2_PLACEMENT_3D('',#14666,#11512,#11513);
#9938=AXIS2_PLACEMENT_3D('',#14669,#11515,#11516);
#9939=AXIS2_PLACEMENT_3D('',#14670,#11517,#11518);
#9940=AXIS2_PLACEMENT_3D('',#14671,#11519,#11520);
#9941=AXIS2_PLACEMENT_3D('',#14673,#11521,#11522);
#9942=AXIS2_PLACEMENT_3D('',#14676,#11524,#11525);
#9943=AXIS2_PLACEMENT_3D('',#14677,#11526,#11527);
#9944=AXIS2_PLACEMENT_3D('',#14678,#11528,#11529);
#9945=AXIS2_PLACEMENT_3D('',#14680,#11530,#11531);
#9946=AXIS2_PLACEMENT_3D('',#14683,#11533,#11534);
#9947=AXIS2_PLACEMENT_3D('',#14684,#11535,#11536);
#9948=AXIS2_PLACEMENT_3D('',#14687,#11537,#11538);
#9949=AXIS2_PLACEMENT_3D('',#14689,#11539,#11540);
#9950=AXIS2_PLACEMENT_3D('',#14690,#11541,#11542);
#9951=AXIS2_PLACEMENT_3D('',#14691,#11543,#11544);
#9952=AXIS2_PLACEMENT_3D('',#14694,#11545,#11546);
#9953=AXIS2_PLACEMENT_3D('',#14696,#11547,#11548);
#9954=AXIS2_PLACEMENT_3D('',#14697,#11549,#11550);
#9955=AXIS2_PLACEMENT_3D('',#14698,#11551,#11552);
#9956=AXIS2_PLACEMENT_3D('',#14701,#11553,#11554);
#9957=AXIS2_PLACEMENT_3D('',#14703,#11555,#11556);
#9958=AXIS2_PLACEMENT_3D('',#14705,#11557,#11558);
#9959=AXIS2_PLACEMENT_3D('',#14706,#11559,#11560);
#9960=AXIS2_PLACEMENT_3D('',#14707,#11561,#11562);
#9961=AXIS2_PLACEMENT_3D('',#14710,#11565,#11566);
#9962=AXIS2_PLACEMENT_3D('',#14713,#11567,#11568);
#9963=AXIS2_PLACEMENT_3D('',#14715,#11569,#11570);
#9964=AXIS2_PLACEMENT_3D('',#14717,#11571,#11572);
#9965=AXIS2_PLACEMENT_3D('',#14718,#11573,#11574);
#9966=AXIS2_PLACEMENT_3D('',#14719,#11575,#11576);
#9967=AXIS2_PLACEMENT_3D('',#14722,#11577,#11578);
#9968=AXIS2_PLACEMENT_3D('',#14724,#11579,#11580);
#9969=AXIS2_PLACEMENT_3D('',#14726,#11581,#11582);
#9970=AXIS2_PLACEMENT_3D('',#14727,#11583,#11584);
#9971=AXIS2_PLACEMENT_3D('',#14728,#11585,#11586);
#9972=AXIS2_PLACEMENT_3D('',#14731,#11587,#11588);
#9973=AXIS2_PLACEMENT_3D('',#14733,#11589,#11590);
#9974=AXIS2_PLACEMENT_3D('',#14735,#11591,#11592);
#9975=AXIS2_PLACEMENT_3D('',#14736,#11593,#11594);
#9976=AXIS2_PLACEMENT_3D('',#14737,#11595,#11596);
#9977=AXIS2_PLACEMENT_3D('',#14740,#11599,#11600);
#9978=AXIS2_PLACEMENT_3D('',#14743,#11601,#11602);
#9979=AXIS2_PLACEMENT_3D('',#14745,#11603,#11604);
#9980=AXIS2_PLACEMENT_3D('',#14746,#11605,#11606);
#9981=AXIS2_PLACEMENT_3D('',#14747,#11607,#11608);
#9982=AXIS2_PLACEMENT_3D('',#14750,#11611,#11612);
#9983=AXIS2_PLACEMENT_3D('',#14753,#11613,#11614);
#9984=AXIS2_PLACEMENT_3D('',#14755,#11615,#11616);
#9985=AXIS2_PLACEMENT_3D('',#14756,#11617,#11618);
#9986=AXIS2_PLACEMENT_3D('',#14757,#11619,#11620);
#9987=AXIS2_PLACEMENT_3D('',#14760,#11623,#11624);
#9988=AXIS2_PLACEMENT_3D('',#14763,#11625,#11626);
#9989=AXIS2_PLACEMENT_3D('',#14765,#11627,#11628);
#9990=AXIS2_PLACEMENT_3D('',#14766,#11629,#11630);
#9991=AXIS2_PLACEMENT_3D('',#14767,#11631,#11632);
#9992=AXIS2_PLACEMENT_3D('',#14770,#11633,#11634);
#9993=AXIS2_PLACEMENT_3D('',#14772,#11635,#11636);
#9994=AXIS2_PLACEMENT_3D('',#14773,#11637,#11638);
#9995=AXIS2_PLACEMENT_3D('',#14774,#11639,#11640);
#9996=AXIS2_PLACEMENT_3D('',#14777,#11643,#11644);
#9997=AXIS2_PLACEMENT_3D('',#14780,#11645,#11646);
#9998=AXIS2_PLACEMENT_3D('',#14782,#11647,#11648);
#9999=AXIS2_PLACEMENT_3D('',#14783,#11649,#11650);
#10000=AXIS2_PLACEMENT_3D('',#14784,#11651,#11652);
#10001=AXIS2_PLACEMENT_3D('',#14787,#11655,#11656);
#10002=AXIS2_PLACEMENT_3D('',#14790,#11657,#11658);
#10003=AXIS2_PLACEMENT_3D('',#14792,#11659,#11660);
#10004=AXIS2_PLACEMENT_3D('',#14793,#11661,#11662);
#10005=AXIS2_PLACEMENT_3D('',#14794,#11663,#11664);
#10006=AXIS2_PLACEMENT_3D('',#14797,#11667,#11668);
#10007=AXIS2_PLACEMENT_3D('',#14800,#11669,#11670);
#10008=AXIS2_PLACEMENT_3D('',#14802,#11671,#11672);
#10009=AXIS2_PLACEMENT_3D('',#14803,#11673,#11674);
#10010=AXIS2_PLACEMENT_3D('',#14804,#11675,#11676);
#10011=AXIS2_PLACEMENT_3D('',#14807,#11677,#11678);
#10012=AXIS2_PLACEMENT_3D('',#14809,#11679,#11680);
#10013=AXIS2_PLACEMENT_3D('',#14810,#11681,#11682);
#10014=AXIS2_PLACEMENT_3D('',#14811,#11683,#11684);
#10015=AXIS2_PLACEMENT_3D('',#14814,#11687,#11688);
#10016=AXIS2_PLACEMENT_3D('',#14817,#11689,#11690);
#10017=AXIS2_PLACEMENT_3D('',#14819,#11691,#11692);
#10018=AXIS2_PLACEMENT_3D('',#14821,#11693,#11694);
#10019=AXIS2_PLACEMENT_3D('',#14822,#11695,#11696);
#10020=AXIS2_PLACEMENT_3D('',#14823,#11697,#11698);
#10021=AXIS2_PLACEMENT_3D('',#14826,#11701,#11702);
#10022=AXIS2_PLACEMENT_3D('',#14829,#11703,#11704);
#10023=AXIS2_PLACEMENT_3D('',#14831,#11705,#11706);
#10024=AXIS2_PLACEMENT_3D('',#14832,#11707,#11708);
#10025=AXIS2_PLACEMENT_3D('',#14833,#11709,#11710);
#10026=AXIS2_PLACEMENT_3D('',#14836,#11711,#11712);
#10027=AXIS2_PLACEMENT_3D('',#14838,#11713,#11714);
#10028=AXIS2_PLACEMENT_3D('',#14840,#11715,#11716);
#10029=AXIS2_PLACEMENT_3D('',#14841,#11717,#11718);
#10030=AXIS2_PLACEMENT_3D('',#14842,#11719,#11720);
#10031=AXIS2_PLACEMENT_3D('',#14845,#11721,#11722);
#10032=AXIS2_PLACEMENT_3D('',#14847,#11723,#11724);
#10033=AXIS2_PLACEMENT_3D('',#14848,#11725,#11726);
#10034=AXIS2_PLACEMENT_3D('',#14849,#11727,#11728);
#10035=AXIS2_PLACEMENT_3D('',#14852,#11729,#11730);
#10036=AXIS2_PLACEMENT_3D('',#14854,#11731,#11732);
#10037=AXIS2_PLACEMENT_3D('',#14855,#11733,#11734);
#10038=AXIS2_PLACEMENT_3D('',#14856,#11735,#11736);
#10039=AXIS2_PLACEMENT_3D('',#14859,#11739,#11740);
#10040=AXIS2_PLACEMENT_3D('',#14862,#11741,#11742);
#10041=AXIS2_PLACEMENT_3D('',#14864,#11743,#11744);
#10042=AXIS2_PLACEMENT_3D('',#14865,#11745,#11746);
#10043=AXIS2_PLACEMENT_3D('',#14866,#11747,#11748);
#10044=AXIS2_PLACEMENT_3D('',#14869,#11749,#11750);
#10045=AXIS2_PLACEMENT_3D('',#14871,#11751,#11752);
#10046=AXIS2_PLACEMENT_3D('',#14872,#11753,#11754);
#10047=AXIS2_PLACEMENT_3D('',#14873,#11755,#11756);
#10048=AXIS2_PLACEMENT_3D('',#14876,#11757,#11758);
#10049=AXIS2_PLACEMENT_3D('',#14878,#11759,#11760);
#10050=AXIS2_PLACEMENT_3D('',#14879,#11761,#11762);
#10051=AXIS2_PLACEMENT_3D('',#14880,#11763,#11764);
#10052=AXIS2_PLACEMENT_3D('',#14883,#11765,#11766);
#10053=AXIS2_PLACEMENT_3D('',#14885,#11767,#11768);
#10054=AXIS2_PLACEMENT_3D('',#14887,#11769,#11770);
#10055=AXIS2_PLACEMENT_3D('',#14888,#11771,#11772);
#10056=AXIS2_PLACEMENT_3D('',#14889,#11773,#11774);
#10057=AXIS2_PLACEMENT_3D('',#14892,#11777,#11778);
#10058=AXIS2_PLACEMENT_3D('',#14895,#11781,#11782);
#10059=AXIS2_PLACEMENT_3D('',#14898,#11783,#11784);
#10060=AXIS2_PLACEMENT_3D('',#14900,#11785,#11786);
#10061=AXIS2_PLACEMENT_3D('',#14902,#11787,#11788);
#10062=AXIS2_PLACEMENT_3D('',#14903,#11789,#11790);
#10063=AXIS2_PLACEMENT_3D('',#14904,#11791,#11792);
#10064=AXIS2_PLACEMENT_3D('',#14907,#11795,#11796);
#10065=AXIS2_PLACEMENT_3D('',#14910,#11799,#11800);
#10066=AXIS2_PLACEMENT_3D('',#14913,#11803,#11804);
#10067=AXIS2_PLACEMENT_3D('',#14916,#11807,#11808);
#10068=AXIS2_PLACEMENT_3D('',#14919,#11811,#11812);
#10069=AXIS2_PLACEMENT_3D('',#14922,#11815,#11816);
#10070=AXIS2_PLACEMENT_3D('',#14925,#11819,#11820);
#10071=AXIS2_PLACEMENT_3D('',#14928,#11823,#11824);
#10072=AXIS2_PLACEMENT_3D('',#14931,#11827,#11828);
#10073=AXIS2_PLACEMENT_3D('',#14934,#11831,#11832);
#10074=AXIS2_PLACEMENT_3D('',#14937,#11835,#11836);
#10075=AXIS2_PLACEMENT_3D('',#14940,#11839,#11840);
#10076=AXIS2_PLACEMENT_3D('',#14943,#11843,#11844);
#10077=AXIS2_PLACEMENT_3D('',#14946,#11847,#11848);
#10078=AXIS2_PLACEMENT_3D('',#14949,#11851,#11852);
#10079=AXIS2_PLACEMENT_3D('',#14952,#11855,#11856);
#10080=AXIS2_PLACEMENT_3D('',#14955,#11859,#11860);
#10081=AXIS2_PLACEMENT_3D('',#14958,#11863,#11864);
#10082=AXIS2_PLACEMENT_3D('',#14961,#11867,#11868);
#10083=AXIS2_PLACEMENT_3D('',#14964,#11871,#11872);
#10084=AXIS2_PLACEMENT_3D('',#14967,#11875,#11876);
#10085=AXIS2_PLACEMENT_3D('',#14970,#11879,#11880);
#10086=AXIS2_PLACEMENT_3D('',#14973,#11883,#11884);
#10087=AXIS2_PLACEMENT_3D('',#14976,#11887,#11888);
#10088=AXIS2_PLACEMENT_3D('',#14977,#11889,#11890);
#10089=AXIS2_PLACEMENT_3D('',#14978,#11891,#11892);
#10090=AXIS2_PLACEMENT_3D('',#14979,#11893,#11894);
#10091=AXIS2_PLACEMENT_3D('',#14980,#11895,#11896);
#10092=AXIS2_PLACEMENT_3D('',#14981,#11897,#11898);
#10093=AXIS2_PLACEMENT_3D('',#14982,#11899,#11900);
#10094=AXIS2_PLACEMENT_3D('',#14983,#11901,#11902);
#10095=AXIS2_PLACEMENT_3D('',#14984,#11903,#11904);
#10096=AXIS2_PLACEMENT_3D('',#14985,#11905,#11906);
#10097=AXIS2_PLACEMENT_3D('',#14986,#11907,#11908);
#10098=AXIS2_PLACEMENT_3D('',#14987,#11909,#11910);
#10099=AXIS2_PLACEMENT_3D('',#14988,#11911,#11912);
#10100=AXIS2_PLACEMENT_3D('',#14989,#11913,#11914);
#10101=AXIS2_PLACEMENT_3D('',#14990,#11915,#11916);
#10102=AXIS2_PLACEMENT_3D('',#14991,#11917,#11918);
#10103=AXIS2_PLACEMENT_3D('',#14993,#11919,#11920);
#10104=AXIS2_PLACEMENT_3D('',#14996,#11922,#11923);
#10105=AXIS2_PLACEMENT_3D('',#14997,#11924,#11925);
#10106=AXIS2_PLACEMENT_3D('',#14998,#11926,#11927);
#10107=AXIS2_PLACEMENT_3D('',#15000,#11928,#11929);
#10108=AXIS2_PLACEMENT_3D('',#15003,#11931,#11932);
#10109=AXIS2_PLACEMENT_3D('',#15004,#11933,#11934);
#10110=AXIS2_PLACEMENT_3D('',#15005,#11935,#11936);
#10111=AXIS2_PLACEMENT_3D('',#15007,#11937,#11938);
#10112=AXIS2_PLACEMENT_3D('',#15010,#11940,#11941);
#10113=AXIS2_PLACEMENT_3D('',#15011,#11942,#11943);
#10114=AXIS2_PLACEMENT_3D('',#15012,#11944,#11945);
#10115=AXIS2_PLACEMENT_3D('',#15014,#11946,#11947);
#10116=AXIS2_PLACEMENT_3D('',#15017,#11949,#11950);
#10117=AXIS2_PLACEMENT_3D('',#15018,#11951,#11952);
#10118=AXIS2_PLACEMENT_3D('',#15019,#11953,#11954);
#10119=AXIS2_PLACEMENT_3D('',#15021,#11955,#11956);
#10120=AXIS2_PLACEMENT_3D('',#15024,#11958,#11959);
#10121=AXIS2_PLACEMENT_3D('',#15025,#11960,#11961);
#10122=AXIS2_PLACEMENT_3D('',#15026,#11962,#11963);
#10123=AXIS2_PLACEMENT_3D('',#15028,#11964,#11965);
#10124=AXIS2_PLACEMENT_3D('',#15031,#11967,#11968);
#10125=AXIS2_PLACEMENT_3D('',#15032,#11969,#11970);
#10126=AXIS2_PLACEMENT_3D('',#15033,#11971,#11972);
#10127=AXIS2_PLACEMENT_3D('',#15035,#11973,#11974);
#10128=AXIS2_PLACEMENT_3D('',#15038,#11976,#11977);
#10129=AXIS2_PLACEMENT_3D('',#15039,#11978,#11979);
#10130=AXIS2_PLACEMENT_3D('',#15040,#11980,#11981);
#10131=AXIS2_PLACEMENT_3D('',#15042,#11982,#11983);
#10132=AXIS2_PLACEMENT_3D('',#15045,#11985,#11986);
#10133=AXIS2_PLACEMENT_3D('',#15046,#11987,#11988);
#10134=AXIS2_PLACEMENT_3D('',#15047,#11989,#11990);
#10135=AXIS2_PLACEMENT_3D('',#15050,#11991,#11992);
#10136=AXIS2_PLACEMENT_3D('',#15058,#11996,#11997);
#10137=AXIS2_PLACEMENT_3D('',#15060,#11999,#12000);
#10138=AXIS2_PLACEMENT_3D('',#15063,#12001,#12002);
#10139=AXIS2_PLACEMENT_3D('',#15067,#12004,#12005);
#10140=AXIS2_PLACEMENT_3D('',#15073,#12009,#12010);
#10141=AXIS2_PLACEMENT_3D('',#15076,#12013,#12014);
#10142=AXIS2_PLACEMENT_3D('',#15080,#12016,#12017);
#10143=AXIS2_PLACEMENT_3D('',#15082,#12019,#12020);
#10144=AXIS2_PLACEMENT_3D('',#15086,#12022,#12023);
#10145=AXIS2_PLACEMENT_3D('',#15088,#12025,#12026);
#10146=AXIS2_PLACEMENT_3D('',#15092,#12029,#12030);
#10147=AXIS2_PLACEMENT_3D('',#15096,#12033,#12034);
#10148=AXIS2_PLACEMENT_3D('',#15098,#12035,#12036);
#10149=AXIS2_PLACEMENT_3D('',#15100,#12038,#12039);
#10150=AXIS2_PLACEMENT_3D('',#15103,#12041,#12042);
#10151=AXIS2_PLACEMENT_3D('',#15104,#12043,#12044);
#10152=AXIS2_PLACEMENT_3D('',#15122,#12053,#12054);
#10153=AXIS2_PLACEMENT_3D('',#15128,#12057,#12058);
#10154=AXIS2_PLACEMENT_3D('',#15132,#12060,#12061);
#10155=AXIS2_PLACEMENT_3D('',#15138,#12064,#12065);
#10156=AXIS2_PLACEMENT_3D('',#15142,#12068,#12069);
#10157=AXIS2_PLACEMENT_3D('',#15144,#12070,#12071);
#10158=AXIS2_PLACEMENT_3D('',#15150,#12074,#12075);
#10159=AXIS2_PLACEMENT_3D('',#15152,#12077,#12078);
#10160=AXIS2_PLACEMENT_3D('',#15154,#12079,#12080);
#10161=AXIS2_PLACEMENT_3D('',#15158,#12082,#12083);
#10162=AXIS2_PLACEMENT_3D('',#15162,#12086,#12087);
#10163=AXIS2_PLACEMENT_3D('',#15164,#12089,#12090);
#10164=AXIS2_PLACEMENT_3D('',#15167,#12092,#12093);
#10165=AXIS2_PLACEMENT_3D('',#15168,#12094,#12095);
#10166=AXIS2_PLACEMENT_3D('',#15174,#12098,#12099);
#10167=AXIS2_PLACEMENT_3D('',#15180,#12102,#12103);
#10168=AXIS2_PLACEMENT_3D('',#15184,#12105,#12106);
#10169=AXIS2_PLACEMENT_3D('',#15190,#12109,#12110);
#10170=AXIS2_PLACEMENT_3D('',#15199,#12116,#12117);
#10171=AXIS2_PLACEMENT_3D('',#15203,#12120,#12121);
#10172=AXIS2_PLACEMENT_3D('',#15206,#12123,#12124);
#10173=AXIS2_PLACEMENT_3D('',#15207,#12125,#12126);
#10174=AXIS2_PLACEMENT_3D('',#15209,#12127,#12128);
#10175=AXIS2_PLACEMENT_3D('',#15211,#12129,#12130);
#10176=AXIS2_PLACEMENT_3D('',#15212,#12131,#12132);
#10177=AXIS2_PLACEMENT_3D('',#15213,#12133,#12134);
#10178=AXIS2_PLACEMENT_3D('',#15215,#12135,#12136);
#10179=AXIS2_PLACEMENT_3D('',#15217,#12137,#12138);
#10180=AXIS2_PLACEMENT_3D('',#15218,#12139,#12140);
#10181=AXIS2_PLACEMENT_3D('',#15219,#12141,#12142);
#10182=AXIS2_PLACEMENT_3D('',#15221,#12143,#12144);
#10183=AXIS2_PLACEMENT_3D('',#15223,#12145,#12146);
#10184=AXIS2_PLACEMENT_3D('',#15224,#12147,#12148);
#10185=AXIS2_PLACEMENT_3D('',#15225,#12149,#12150);
#10186=AXIS2_PLACEMENT_3D('',#15227,#12151,#12152);
#10187=AXIS2_PLACEMENT_3D('',#15229,#12153,#12154);
#10188=AXIS2_PLACEMENT_3D('',#15230,#12155,#12156);
#10189=AXIS2_PLACEMENT_3D('',#15231,#12157,#12158);
#10190=AXIS2_PLACEMENT_3D('',#15233,#12160,#12161);
#10191=AXIS2_PLACEMENT_3D('',#15235,#12162,#12163);
#10192=AXIS2_PLACEMENT_3D('',#15237,#12164,#12165);
#10193=AXIS2_PLACEMENT_3D('',#15238,#12166,#12167);
#10194=AXIS2_PLACEMENT_3D('',#15239,#12168,#12169);
#10195=AXIS2_PLACEMENT_3D('',#15241,#12171,#12172);
#10196=AXIS2_PLACEMENT_3D('',#15244,#12175,#12176);
#10197=AXIS2_PLACEMENT_3D('',#15246,#12177,#12178);
#10198=AXIS2_PLACEMENT_3D('',#15248,#12179,#12180);
#10199=AXIS2_PLACEMENT_3D('',#15249,#12181,#12182);
#10200=AXIS2_PLACEMENT_3D('',#15250,#12183,#12184);
#10201=AXIS2_PLACEMENT_3D('',#15253,#12187,#12188);
#10202=AXIS2_PLACEMENT_3D('',#15255,#12190,#12191);
#10203=AXIS2_PLACEMENT_3D('',#15257,#12192,#12193);
#10204=AXIS2_PLACEMENT_3D('',#15259,#12194,#12195);
#10205=AXIS2_PLACEMENT_3D('',#15260,#12196,#12197);
#10206=AXIS2_PLACEMENT_3D('',#15261,#12198,#12199);
#10207=AXIS2_PLACEMENT_3D('',#15263,#12200,#12201);
#10208=AXIS2_PLACEMENT_3D('',#15264,#12202,#12203);
#10209=AXIS2_PLACEMENT_3D('',#15265,#12204,#12205);
#10210=AXIS2_PLACEMENT_3D('',#15267,#12206,#12207);
#10211=AXIS2_PLACEMENT_3D('',#15269,#12208,#12209);
#10212=AXIS2_PLACEMENT_3D('',#15270,#12210,#12211);
#10213=AXIS2_PLACEMENT_3D('',#15271,#12212,#12213);
#10214=AXIS2_PLACEMENT_3D('',#15273,#12215,#12216);
#10215=AXIS2_PLACEMENT_3D('',#15276,#12219,#12220);
#10216=AXIS2_PLACEMENT_3D('',#15278,#12221,#12222);
#10217=AXIS2_PLACEMENT_3D('',#15279,#12223,#12224);
#10218=AXIS2_PLACEMENT_3D('',#15280,#12225,#12226);
#10219=AXIS2_PLACEMENT_3D('',#15282,#12227,#12228);
#10220=AXIS2_PLACEMENT_3D('',#15284,#12229,#12230);
#10221=AXIS2_PLACEMENT_3D('',#15285,#12231,#12232);
#10222=AXIS2_PLACEMENT_3D('',#15286,#12233,#12234);
#10223=AXIS2_PLACEMENT_3D('',#15288,#12235,#12236);
#10224=AXIS2_PLACEMENT_3D('',#15290,#12237,#12238);
#10225=AXIS2_PLACEMENT_3D('',#15291,#12239,#12240);
#10226=AXIS2_PLACEMENT_3D('',#15292,#12241,#12242);
#10227=AXIS2_PLACEMENT_3D('',#15294,#12244,#12245);
#10228=AXIS2_PLACEMENT_3D('',#15297,#12248,#12249);
#10229=AXIS2_PLACEMENT_3D('',#15299,#12250,#12251);
#10230=AXIS2_PLACEMENT_3D('',#15301,#12252,#12253);
#10231=AXIS2_PLACEMENT_3D('',#15302,#12254,#12255);
#10232=AXIS2_PLACEMENT_3D('',#15303,#12256,#12257);
#10233=AXIS2_PLACEMENT_3D('',#15305,#12258,#12259);
#10234=AXIS2_PLACEMENT_3D('',#15307,#12260,#12261);
#10235=AXIS2_PLACEMENT_3D('',#15308,#12262,#12263);
#10236=AXIS2_PLACEMENT_3D('',#15309,#12264,#12265);
#10237=AXIS2_PLACEMENT_3D('',#15311,#12267,#12268);
#10238=AXIS2_PLACEMENT_3D('',#15313,#12269,#12270);
#10239=AXIS2_PLACEMENT_3D('',#15315,#12271,#12272);
#10240=AXIS2_PLACEMENT_3D('',#15316,#12273,#12274);
#10241=AXIS2_PLACEMENT_3D('',#15317,#12275,#12276);
#10242=AXIS2_PLACEMENT_3D('',#15319,#12278,#12279);
#10243=AXIS2_PLACEMENT_3D('',#15322,#12282,#12283);
#10244=AXIS2_PLACEMENT_3D('',#15324,#12284,#12285);
#10245=AXIS2_PLACEMENT_3D('',#15325,#12286,#12287);
#10246=AXIS2_PLACEMENT_3D('',#15326,#12288,#12289);
#10247=AXIS2_PLACEMENT_3D('',#15329,#12292,#12293);
#10248=AXIS2_PLACEMENT_3D('',#15331,#12295,#12296);
#10249=AXIS2_PLACEMENT_3D('',#15333,#12297,#12298);
#10250=AXIS2_PLACEMENT_3D('',#15335,#12299,#12300);
#10251=AXIS2_PLACEMENT_3D('',#15336,#12301,#12302);
#10252=AXIS2_PLACEMENT_3D('',#15337,#12303,#12304);
#10253=AXIS2_PLACEMENT_3D('',#15339,#12305,#12306);
#10254=AXIS2_PLACEMENT_3D('',#15340,#12307,#12308);
#10255=AXIS2_PLACEMENT_3D('',#15341,#12309,#12310);
#10256=AXIS2_PLACEMENT_3D('',#15343,#12312,#12313);
#10257=AXIS2_PLACEMENT_3D('',#15345,#12314,#12315);
#10258=AXIS2_PLACEMENT_3D('',#15347,#12316,#12317);
#10259=AXIS2_PLACEMENT_3D('',#15348,#12318,#12319);
#10260=AXIS2_PLACEMENT_3D('',#15349,#12320,#12321);
#10261=AXIS2_PLACEMENT_3D('',#15351,#12322,#12323);
#10262=AXIS2_PLACEMENT_3D('',#15352,#12324,#12325);
#10263=AXIS2_PLACEMENT_3D('',#15353,#12326,#12327);
#10264=AXIS2_PLACEMENT_3D('',#15354,#12328,#12329);
#10265=AXIS2_PLACEMENT_3D('',#15355,#12330,#12331);
#10266=AXIS2_PLACEMENT_3D('',#15358,#12332,#12333);
#10267=AXIS2_PLACEMENT_3D('',#15359,#12334,#12335);
#10268=AXIS2_PLACEMENT_3D('',#15360,#12336,#12337);
#10269=AXIS2_PLACEMENT_3D('',#15361,#12338,#12339);
#10270=AXIS2_PLACEMENT_3D('',#15363,#12341,#12342);
#10271=AXIS2_PLACEMENT_3D('',#15365,#12344,#12345);
#10272=AXIS2_PLACEMENT_3D('',#15367,#12346,#12347);
#10273=AXIS2_PLACEMENT_3D('',#15369,#12348,#12349);
#10274=AXIS2_PLACEMENT_3D('',#15370,#12350,#12351);
#10275=AXIS2_PLACEMENT_3D('',#15371,#12352,#12353);
#10276=AXIS2_PLACEMENT_3D('',#15374,#12356,#12357);
#10277=AXIS2_PLACEMENT_3D('',#15376,#12359,#12360);
#10278=AXIS2_PLACEMENT_3D('',#15378,#12362,#12363);
#10279=AXIS2_PLACEMENT_3D('',#15380,#12365,#12366);
#10280=AXIS2_PLACEMENT_3D('',#15382,#12368,#12369);
#10281=AXIS2_PLACEMENT_3D('',#15385,#12372,#12373);
#10282=AXIS2_PLACEMENT_3D('',#15387,#12375,#12376);
#10283=AXIS2_PLACEMENT_3D('',#15389,#12378,#12379);
#10284=AXIS2_PLACEMENT_3D('',#15391,#12381,#12382);
#10285=AXIS2_PLACEMENT_3D('',#15393,#12384,#12385);
#10286=AXIS2_PLACEMENT_3D('',#15395,#12387,#12388);
#10287=AXIS2_PLACEMENT_3D('',#15397,#12390,#12391);
#10288=AXIS2_PLACEMENT_3D('',#15399,#12393,#12394);
#10289=AXIS2_PLACEMENT_3D('',#15401,#12396,#12397);
#10290=AXIS2_PLACEMENT_3D('',#15404,#12400,#12401);
#10291=AXIS2_PLACEMENT_3D('',#15405,#12402,#12403);
#10292=AXIS2_PLACEMENT_3D('',#15406,#12404,#12405);
#10293=AXIS2_PLACEMENT_3D('',#15407,#12406,#12407);
#10294=AXIS2_PLACEMENT_3D('',#15408,#12408,#12409);
#10295=AXIS2_PLACEMENT_3D('',#15409,#12410,#12411);
#10296=AXIS2_PLACEMENT_3D('',#15410,#12412,#12413);
#10297=AXIS2_PLACEMENT_3D('',#15411,#12414,#12415);
#10298=AXIS2_PLACEMENT_3D('',#15412,#12416,#12417);
#10299=AXIS2_PLACEMENT_3D('',#15413,#12418,#12419);
#10300=AXIS2_PLACEMENT_3D('',#15414,#12420,#12421);
#10301=AXIS2_PLACEMENT_3D('',#15415,#12422,#12423);
#10302=AXIS2_PLACEMENT_3D('',#15416,#12424,#12425);
#10303=AXIS2_PLACEMENT_3D('',#15419,#12426,#12427);
#10304=AXIS2_PLACEMENT_3D('',#15423,#12429,#12430);
#10305=AXIS2_PLACEMENT_3D('',#15425,#12432,#12433);
#10306=AXIS2_PLACEMENT_3D('',#15428,#12434,#12435);
#10307=AXIS2_PLACEMENT_3D('',#15429,#12436,#12437);
#10308=AXIS2_PLACEMENT_3D('',#15430,#12438,#12439);
#10309=AXIS2_PLACEMENT_3D('',#15431,#12440,#12441);
#10310=AXIS2_PLACEMENT_3D('',#15434,#12442,#12443);
#10311=AXIS2_PLACEMENT_3D('',#15437,#12446,#12447);
#10312=AXIS2_PLACEMENT_3D('',#15438,#12448,#12449);
#10313=AXIS2_PLACEMENT_3D('',#15439,#12450,#12451);
#10314=AXIS2_PLACEMENT_3D('',#15440,#12452,#12453);
#10315=AXIS2_PLACEMENT_3D('',#15444,#12455,#12456);
#10316=AXIS2_PLACEMENT_3D('',#15446,#12458,#12459);
#10317=AXIS2_PLACEMENT_3D('',#15450,#12462,#12463);
#10318=AXIS2_PLACEMENT_3D('',#15459,#12468,#12469);
#10319=AXIS2_PLACEMENT_3D('',#15461,#12470,#12471);
#10320=AXIS2_PLACEMENT_3D('',#15463,#12472,#12473);
#10321=AXIS2_PLACEMENT_3D('',#15465,#12474,#12475);
#10322=AXIS2_PLACEMENT_3D('',#15466,#12476,#12477);
#10323=AXIS2_PLACEMENT_3D('',#15467,#12478,#12479);
#10324=AXIS2_PLACEMENT_3D('',#15470,#12480,#12481);
#10325=AXIS2_PLACEMENT_3D('',#15472,#12482,#12483);
#10326=AXIS2_PLACEMENT_3D('',#15473,#12484,#12485);
#10327=AXIS2_PLACEMENT_3D('',#15474,#12486,#12487);
#10328=AXIS2_PLACEMENT_3D('',#15477,#12488,#12489);
#10329=AXIS2_PLACEMENT_3D('',#15478,#12490,#12491);
#10330=AXIS2_PLACEMENT_3D('',#15480,#12492,#12493);
#10331=AXIS2_PLACEMENT_3D('',#15481,#12494,#12495);
#10332=AXIS2_PLACEMENT_3D('',#15482,#12496,#12497);
#10333=AXIS2_PLACEMENT_3D('',#15486,#12499,#12500);
#10334=AXIS2_PLACEMENT_3D('',#15488,#12502,#12503);
#10335=AXIS2_PLACEMENT_3D('',#15491,#12504,#12505);
#10336=AXIS2_PLACEMENT_3D('',#15492,#12506,#12507);
#10337=AXIS2_PLACEMENT_3D('',#15493,#12508,#12509);
#10338=AXIS2_PLACEMENT_3D('',#15494,#12510,#12511);
#10339=AXIS2_PLACEMENT_3D('',#15497,#12512,#12513);
#10340=AXIS2_PLACEMENT_3D('',#15499,#12514,#12515);
#10341=AXIS2_PLACEMENT_3D('',#15500,#12516,#12517);
#10342=AXIS2_PLACEMENT_3D('',#15501,#12518,#12519);
#10343=AXIS2_PLACEMENT_3D('',#15504,#12522,#12523);
#10344=AXIS2_PLACEMENT_3D('',#15507,#12524,#12525);
#10345=AXIS2_PLACEMENT_3D('',#15509,#12526,#12527);
#10346=AXIS2_PLACEMENT_3D('',#15510,#12528,#12529);
#10347=AXIS2_PLACEMENT_3D('',#15511,#12530,#12531);
#10348=AXIS2_PLACEMENT_3D('',#15513,#12532,#12533);
#10349=AXIS2_PLACEMENT_3D('',#15515,#12534,#12535);
#10350=AXIS2_PLACEMENT_3D('',#15516,#12536,#12537);
#10351=AXIS2_PLACEMENT_3D('',#15517,#12538,#12539);
#10352=AXIS2_PLACEMENT_3D('',#15520,#12540,#12541);
#10353=AXIS2_PLACEMENT_3D('',#15522,#12542,#12543);
#10354=AXIS2_PLACEMENT_3D('',#15523,#12544,#12545);
#10355=AXIS2_PLACEMENT_3D('',#15524,#12546,#12547);
#10356=AXIS2_PLACEMENT_3D('',#15527,#12548,#12549);
#10357=AXIS2_PLACEMENT_3D('',#15529,#12550,#12551);
#10358=AXIS2_PLACEMENT_3D('',#15530,#12552,#12553);
#10359=AXIS2_PLACEMENT_3D('',#15531,#12554,#12555);
#10360=AXIS2_PLACEMENT_3D('',#15534,#12558,#12559);
#10361=AXIS2_PLACEMENT_3D('',#15537,#12560,#12561);
#10362=AXIS2_PLACEMENT_3D('',#15539,#12562,#12563);
#10363=AXIS2_PLACEMENT_3D('',#15540,#12564,#12565);
#10364=AXIS2_PLACEMENT_3D('',#15541,#12566,#12567);
#10365=AXIS2_PLACEMENT_3D('',#15544,#12570,#12571);
#10366=AXIS2_PLACEMENT_3D('',#15547,#12574,#12575);
#10367=AXIS2_PLACEMENT_3D('',#15550,#12578,#12579);
#10368=AXIS2_PLACEMENT_3D('',#15553,#12582,#12583);
#10369=AXIS2_PLACEMENT_3D('',#15556,#12586,#12587);
#10370=AXIS2_PLACEMENT_3D('',#15559,#12590,#12591);
#10371=AXIS2_PLACEMENT_3D('',#15561,#12593,#12594);
#10372=AXIS2_PLACEMENT_3D('',#15563,#12596,#12597);
#10373=AXIS2_PLACEMENT_3D('',#15566,#12600,#12601);
#10374=AXIS2_PLACEMENT_3D('',#15569,#12604,#12605);
#10375=AXIS2_PLACEMENT_3D('',#15571,#12607,#12608);
#10376=AXIS2_PLACEMENT_3D('',#15573,#12610,#12611);
#10377=AXIS2_PLACEMENT_3D('',#15577,#12613,#12614);
#10378=AXIS2_PLACEMENT_3D('',#15579,#12616,#12617);
#10379=AXIS2_PLACEMENT_3D('',#15582,#12620,#12621);
#10380=AXIS2_PLACEMENT_3D('',#15584,#12623,#12624);
#10381=AXIS2_PLACEMENT_3D('',#15585,#12625,#12626);
#10382=AXIS2_PLACEMENT_3D('',#15586,#12627,#12628);
#10383=AXIS2_PLACEMENT_3D('',#15591,#12630,#12631);
#10384=AXIS2_PLACEMENT_3D('',#15594,#12633,#12634);
#10385=AXIS2_PLACEMENT_3D('',#15595,#12635,#12636);
#10386=AXIS2_PLACEMENT_3D('',#15596,#12637,#12638);
#10387=AXIS2_PLACEMENT_3D('',#15597,#12639,#12640);
#10388=AXIS2_PLACEMENT_3D('',#15598,#12641,#12642);
#10389=AXIS2_PLACEMENT_3D('',#15599,#12643,#12644);
#10390=AXIS2_PLACEMENT_3D('',#15600,#12645,#12646);
#10391=AXIS2_PLACEMENT_3D('',#15602,#12647,#12648);
#10392=AXIS2_PLACEMENT_3D('',#15603,#12649,#12650);
#10393=AXIS2_PLACEMENT_3D('',#15604,#12651,#12652);
#10394=AXIS2_PLACEMENT_3D('',#15605,#12653,#12654);
#10395=AXIS2_PLACEMENT_3D('',#15607,#12656,#12657);
#10396=AXIS2_PLACEMENT_3D('',#15608,#12658,#12659);
#10397=AXIS2_PLACEMENT_3D('',#15610,#12661,#12662);
#10398=AXIS2_PLACEMENT_3D('',#15611,#12663,#12664);
#10399=AXIS2_PLACEMENT_3D('',#15612,#12665,#12666);
#10400=AXIS2_PLACEMENT_3D('',#15613,#12667,#12668);
#10401=AXIS2_PLACEMENT_3D('',#15615,#12669,#12670);
#10402=AXIS2_PLACEMENT_3D('',#15618,#12672,#12673);
#10403=AXIS2_PLACEMENT_3D('',#15619,#12674,#12675);
#10404=AXIS2_PLACEMENT_3D('',#15621,#12676,#12677);
#10405=AXIS2_PLACEMENT_3D('',#15625,#12679,#12680);
#10406=AXIS2_PLACEMENT_3D('',#15651,#12682,#12683);
#10407=AXIS2_PLACEMENT_3D('',#15676,#12685,#12686);
#10408=AXIS2_PLACEMENT_3D('',#15677,#12687,#12688);
#10409=AXIS2_PLACEMENT_3D('',#15685,#12692,#12693);
#10410=AXIS2_PLACEMENT_3D('',#15689,#12695,#12696);
#10411=AXIS2_PLACEMENT_3D('',#15693,#12698,#12699);
#10412=AXIS2_PLACEMENT_3D('',#15697,#12701,#12702);
#10413=AXIS2_PLACEMENT_3D('',#15705,#12706,#12707);
#10414=AXIS2_PLACEMENT_3D('',#15709,#12709,#12710);
#10415=AXIS2_PLACEMENT_3D('',#15711,#12711,#12712);
#10416=AXIS2_PLACEMENT_3D('',#15715,#12714,#12715);
#10417=AXIS2_PLACEMENT_3D('',#15717,#12716,#12717);
#10418=AXIS2_PLACEMENT_3D('',#15721,#12719,#12720);
#10419=AXIS2_PLACEMENT_3D('',#15723,#12721,#12722);
#10420=AXIS2_PLACEMENT_3D('',#15725,#12724,#12725);
#10421=AXIS2_PLACEMENT_3D('',#15728,#12727,#12728);
#10422=AXIS2_PLACEMENT_3D('',#15729,#12729,#12730);
#10423=AXIS2_PLACEMENT_3D('',#15733,#12733,#12734);
#10424=AXIS2_PLACEMENT_3D('',#15736,#12736,#12737);
#10425=AXIS2_PLACEMENT_3D('',#15737,#12738,#12739);
#10426=AXIS2_PLACEMENT_3D('',#15739,#12740,#12741);
#10427=AXIS2_PLACEMENT_3D('',#15766,#12744,#12745);
#10428=AXIS2_PLACEMENT_3D('',#15790,#12747,#12748);
#10429=AXIS2_PLACEMENT_3D('',#15792,#12749,#12750);
#10430=AXIS2_PLACEMENT_3D('',#15795,#12752,#12753);
#10431=AXIS2_PLACEMENT_3D('',#15796,#12754,#12755);
#10432=AXIS2_PLACEMENT_3D('',#15798,#12756,#12757);
#10433=AXIS2_PLACEMENT_3D('',#15801,#12759,#12760);
#10434=AXIS2_PLACEMENT_3D('',#15802,#12761,#12762);
#10435=AXIS2_PLACEMENT_3D('',#15804,#12763,#12764);
#10436=AXIS2_PLACEMENT_3D('',#15808,#12766,#12767);
#10437=AXIS2_PLACEMENT_3D('',#15856,#12770,#12771);
#10438=AXIS2_PLACEMENT_3D('',#15857,#12772,#12773);
#10439=AXIS2_PLACEMENT_3D('',#15859,#12774,#12775);
#10440=AXIS2_PLACEMENT_3D('',#15862,#12777,#12778);
#10441=AXIS2_PLACEMENT_3D('',#15863,#12779,#12780);
#10442=AXIS2_PLACEMENT_3D('',#15865,#12781,#12782);
#10443=AXIS2_PLACEMENT_3D('',#15869,#12784,#12785);
#10444=AXIS2_PLACEMENT_3D('',#15917,#12788,#12789);
#10445=AXIS2_PLACEMENT_3D('',#15918,#12790,#12791);
#10446=AXIS2_PLACEMENT_3D('',#15920,#12792,#12793);
#10447=AXIS2_PLACEMENT_3D('',#15923,#12795,#12796);
#10448=AXIS2_PLACEMENT_3D('',#15924,#12797,#12798);
#10449=AXIS2_PLACEMENT_3D('',#15926,#12799,#12800);
#10450=AXIS2_PLACEMENT_3D('',#15930,#12802,#12803);
#10451=AXIS2_PLACEMENT_3D('',#15978,#12806,#12807);
#10452=AXIS2_PLACEMENT_3D('',#15979,#12808,#12809);
#10453=AXIS2_PLACEMENT_3D('',#15981,#12810,#12811);
#10454=AXIS2_PLACEMENT_3D('',#15984,#12813,#12814);
#10455=AXIS2_PLACEMENT_3D('',#15985,#12815,#12816);
#10456=AXIS2_PLACEMENT_3D('',#15987,#12817,#12818);
#10457=AXIS2_PLACEMENT_3D('',#16014,#12821,#12822);
#10458=AXIS2_PLACEMENT_3D('',#16038,#12824,#12825);
#10459=AXIS2_PLACEMENT_3D('',#16040,#12826,#12827);
#10460=AXIS2_PLACEMENT_3D('',#16043,#12829,#12830);
#10461=AXIS2_PLACEMENT_3D('',#16044,#12831,#12832);
#10462=AXIS2_PLACEMENT_3D('',#16046,#12833,#12834);
#10463=AXIS2_PLACEMENT_3D('',#16050,#12836,#12837);
#10464=AXIS2_PLACEMENT_3D('',#16098,#12840,#12841);
#10465=AXIS2_PLACEMENT_3D('',#16099,#12842,#12843);
#10466=AXIS2_PLACEMENT_3D('',#16101,#12844,#12845);
#10467=AXIS2_PLACEMENT_3D('',#16105,#12847,#12848);
#10468=AXIS2_PLACEMENT_3D('',#16131,#12850,#12851);
#10469=AXIS2_PLACEMENT_3D('',#16157,#12853,#12854);
#10470=AXIS2_PLACEMENT_3D('',#16181,#12855,#12856);
#10471=AXIS2_PLACEMENT_3D('',#16200,#12857,#12858);
#10472=AXIS2_PLACEMENT_3D('',#16219,#12859,#12860);
#10473=AXIS2_PLACEMENT_3D('',#16242,#12861,#12862);
#10474=AXIS2_PLACEMENT_3D('',#16243,#12863,#12864);
#10475=AXIS2_PLACEMENT_3D('',#16245,#12865,#12866);
#10476=AXIS2_PLACEMENT_3D('',#16249,#12868,#12869);
#10477=AXIS2_PLACEMENT_3D('',#16297,#12872,#12873);
#10478=AXIS2_PLACEMENT_3D('',#16298,#12874,#12875);
#10479=AXIS2_PLACEMENT_3D('',#16300,#12876,#12877);
#10480=AXIS2_PLACEMENT_3D('',#16304,#12879,#12880);
#10481=AXIS2_PLACEMENT_3D('',#16330,#12882,#12883);
#10482=AXIS2_PLACEMENT_3D('',#16356,#12885,#12886);
#10483=AXIS2_PLACEMENT_3D('',#16380,#12887,#12888);
#10484=AXIS2_PLACEMENT_3D('',#16399,#12889,#12890);
#10485=AXIS2_PLACEMENT_3D('',#16418,#12891,#12892);
#10486=AXIS2_PLACEMENT_3D('',#16441,#12893,#12894);
#10487=AXIS2_PLACEMENT_3D('',#16442,#12895,#12896);
#10488=AXIS2_PLACEMENT_3D('',#16444,#12897,#12898);
#10489=AXIS2_PLACEMENT_3D('',#16448,#12900,#12901);
#10490=AXIS2_PLACEMENT_3D('',#16474,#12903,#12904);
#10491=AXIS2_PLACEMENT_3D('',#16500,#12906,#12907);
#10492=AXIS2_PLACEMENT_3D('',#16524,#12908,#12909);
#10493=AXIS2_PLACEMENT_3D('',#16543,#12910,#12911);
#10494=AXIS2_PLACEMENT_3D('',#16562,#12912,#12913);
#10495=AXIS2_PLACEMENT_3D('',#16585,#12914,#12915);
#10496=AXIS2_PLACEMENT_3D('',#16586,#12916,#12917);
#10497=AXIS2_PLACEMENT_3D('',#16588,#12918,#12919);
#10498=AXIS2_PLACEMENT_3D('',#16592,#12921,#12922);
#10499=AXIS2_PLACEMENT_3D('',#16618,#12924,#12925);
#10500=AXIS2_PLACEMENT_3D('',#16644,#12927,#12928);
#10501=AXIS2_PLACEMENT_3D('',#16668,#12929,#12930);
#10502=AXIS2_PLACEMENT_3D('',#16687,#12931,#12932);
#10503=AXIS2_PLACEMENT_3D('',#16706,#12933,#12934);
#10504=AXIS2_PLACEMENT_3D('',#16729,#12935,#12936);
#10505=AXIS2_PLACEMENT_3D('',#16730,#12937,#12938);
#10506=AXIS2_PLACEMENT_3D('',#16732,#12939,#12940);
#10507=AXIS2_PLACEMENT_3D('',#16735,#12942,#12943);
#10508=AXIS2_PLACEMENT_3D('',#16736,#12944,#12945);
#10509=AXIS2_PLACEMENT_3D('',#16738,#12946,#12947);
#10510=AXIS2_PLACEMENT_3D('',#16765,#12950,#12951);
#10511=AXIS2_PLACEMENT_3D('',#16789,#12953,#12954);
#10512=AXIS2_PLACEMENT_3D('',#16791,#12956,#12957);
#10513=AXIS2_PLACEMENT_3D('',#16793,#12958,#12959);
#10514=AXIS2_PLACEMENT_3D('',#16795,#12961,#12962);
#10515=AXIS2_PLACEMENT_3D('',#16797,#12964,#12965);
#10516=AXIS2_PLACEMENT_3D('',#16800,#12967,#12968);
#10517=AXIS2_PLACEMENT_3D('',#16801,#12969,#12970);
#10518=AXIS2_PLACEMENT_3D('',#16803,#12972,#12973);
#10519=AXIS2_PLACEMENT_3D('',#16807,#12976,#12977);
#10520=AXIS2_PLACEMENT_3D('',#16809,#12979,#12980);
#10521=AXIS2_PLACEMENT_3D('',#16813,#12983,#12984);
#10522=AXIS2_PLACEMENT_3D('',#16815,#12986,#12987);
#10523=AXIS2_PLACEMENT_3D('',#16817,#12989,#12990);
#10524=AXIS2_PLACEMENT_3D('',#16819,#12991,#12992);
#10525=AXIS2_PLACEMENT_3D('',#16821,#12994,#12995);
#10526=AXIS2_PLACEMENT_3D('',#16823,#12997,#12998);
#10527=AXIS2_PLACEMENT_3D('',#16826,#13000,#13001);
#10528=AXIS2_PLACEMENT_3D('',#16827,#13002,#13003);
#10529=AXIS2_PLACEMENT_3D('',#16831,#13005,#13006);
#10530=AXIS2_PLACEMENT_3D('',#16833,#13008,#13009);
#10531=AXIS2_PLACEMENT_3D('',#16836,#13012,#13013);
#10532=AXIS2_PLACEMENT_3D('',#16840,#13015,#13016);
#10533=AXIS2_PLACEMENT_3D('',#16842,#13018,#13019);
#10534=AXIS2_PLACEMENT_3D('',#16845,#13022,#13023);
#10535=AXIS2_PLACEMENT_3D('',#16848,#13026,#13027);
#10536=AXIS2_PLACEMENT_3D('',#16852,#13030,#13031);
#10537=AXIS2_PLACEMENT_3D('',#16854,#13033,#13034);
#10538=AXIS2_PLACEMENT_3D('',#16858,#13037,#13038);
#10539=AXIS2_PLACEMENT_3D('',#16860,#13040,#13041);
#10540=AXIS2_PLACEMENT_3D('',#16862,#13043,#13044);
#10541=AXIS2_PLACEMENT_3D('',#16866,#13046,#13047);
#10542=AXIS2_PLACEMENT_3D('',#16868,#13049,#13050);
#10543=AXIS2_PLACEMENT_3D('',#16871,#13053,#13054);
#10544=AXIS2_PLACEMENT_3D('',#16875,#13056,#13057);
#10545=AXIS2_PLACEMENT_3D('',#16877,#13059,#13060);
#10546=AXIS2_PLACEMENT_3D('',#16880,#13063,#13064);
#10547=AXIS2_PLACEMENT_3D('',#16882,#13065,#13066);
#10548=AXIS2_PLACEMENT_3D('',#16884,#13068,#13069);
#10549=AXIS2_PLACEMENT_3D('',#16886,#13071,#13072);
#10550=AXIS2_PLACEMENT_3D('',#16889,#13074,#13075);
#10551=AXIS2_PLACEMENT_3D('',#16890,#13076,#13077);
#10552=AXIS2_PLACEMENT_3D('',#16892,#13079,#13080);
#10553=AXIS2_PLACEMENT_3D('',#16894,#13082,#13083);
#10554=AXIS2_PLACEMENT_3D('',#16898,#13086,#13087);
#10555=AXIS2_PLACEMENT_3D('',#16900,#13089,#13090);
#10556=AXIS2_PLACEMENT_3D('',#16904,#13093,#13094);
#10557=AXIS2_PLACEMENT_3D('',#16906,#13096,#13097);
#10558=AXIS2_PLACEMENT_3D('',#16910,#13100,#13101);
#10559=AXIS2_PLACEMENT_3D('',#16914,#13104,#13105);
#10560=AXIS2_PLACEMENT_3D('',#16916,#13107,#13108);
#10561=AXIS2_PLACEMENT_3D('',#16918,#13110,#13111);
#10562=AXIS2_PLACEMENT_3D('',#16919,#13112,#13113);
#10563=AXIS2_PLACEMENT_3D('',#16920,#13114,#13115);
#10564=AXIS2_PLACEMENT_3D('',#16921,#13116,#13117);
#10565=AXIS2_PLACEMENT_3D('',#16922,#13118,#13119);
#10566=AXIS2_PLACEMENT_3D('',#16923,#13120,#13121);
#10567=AXIS2_PLACEMENT_3D('',#16924,#13122,#13123);
#10568=AXIS2_PLACEMENT_3D('',#16936,#13132,#13133);
#10569=AXIS2_PLACEMENT_3D('',#16938,#13135,#13136);
#10570=AXIS2_PLACEMENT_3D('',#16941,#13138,#13139);
#10571=AXIS2_PLACEMENT_3D('',#16942,#13140,#13141);
#10572=AXIS2_PLACEMENT_3D('',#16944,#13143,#13144);
#10573=AXIS2_PLACEMENT_3D('',#16946,#13146,#13147);
#10574=AXIS2_PLACEMENT_3D('',#16948,#13149,#13150);
#10575=AXIS2_PLACEMENT_3D('',#16952,#13153,#13154);
#10576=AXIS2_PLACEMENT_3D('',#16954,#13156,#13157);
#10577=AXIS2_PLACEMENT_3D('',#16956,#13159,#13160);
#10578=AXIS2_PLACEMENT_3D('',#16958,#13162,#13163);
#10579=AXIS2_PLACEMENT_3D('',#16959,#13164,#13165);
#10580=AXIS2_PLACEMENT_3D('',#16960,#13166,#13167);
#10581=AXIS2_PLACEMENT_3D('',#16961,#13168,#13169);
#10582=AXIS2_PLACEMENT_3D('',#16962,#13170,#13171);
#10583=AXIS2_PLACEMENT_3D('',#16963,#13172,#13173);
#10584=AXIS2_PLACEMENT_3D('',#16967,#13177,#13178);
#10585=AXIS2_PLACEMENT_3D('',#16974,#13183,#13184);
#10586=AXIS2_PLACEMENT_3D('',#16976,#13185,#13186);
#10587=AXIS2_PLACEMENT_3D('',#16977,#13187,#13188);
#10588=AXIS2_PLACEMENT_3D('',#16978,#13189,#13190);
#10589=AXIS2_PLACEMENT_3D('',#16980,#13191,#13192);
#10590=AXIS2_PLACEMENT_3D('',#16981,#13193,#13194);
#10591=AXIS2_PLACEMENT_3D('',#16982,#13195,#13196);
#10592=AXIS2_PLACEMENT_3D('',#16984,#13197,#13198);
#10593=AXIS2_PLACEMENT_3D('',#16986,#13199,#13200);
#10594=AXIS2_PLACEMENT_3D('',#16987,#13201,#13202);
#10595=AXIS2_PLACEMENT_3D('',#16988,#13203,#13204);
#10596=AXIS2_PLACEMENT_3D('',#16990,#13206,#13207);
#10597=AXIS2_PLACEMENT_3D('',#16993,#13208,#13209);
#10598=AXIS2_PLACEMENT_3D('',#16994,#13210,#13211);
#10599=AXIS2_PLACEMENT_3D('',#16995,#13212,#13213);
#10600=AXIS2_PLACEMENT_3D('',#16996,#13214,#13215);
#10601=AXIS2_PLACEMENT_3D('',#16998,#13216,#13217);
#10602=AXIS2_PLACEMENT_3D('',#17000,#13218,#13219);
#10603=AXIS2_PLACEMENT_3D('',#17001,#13220,#13221);
#10604=AXIS2_PLACEMENT_3D('',#17002,#13222,#13223);
#10605=AXIS2_PLACEMENT_3D('',#17005,#13224,#13225);
#10606=AXIS2_PLACEMENT_3D('',#17006,#13226,#13227);
#10607=AXIS2_PLACEMENT_3D('',#17007,#13228,#13229);
#10608=AXIS2_PLACEMENT_3D('',#17008,#13230,#13231);
#10609=AXIS2_PLACEMENT_3D('',#17010,#13233,#13234);
#10610=AXIS2_PLACEMENT_3D('',#17012,#13235,#13236);
#10611=AXIS2_PLACEMENT_3D('',#17013,#13237,#13238);
#10612=AXIS2_PLACEMENT_3D('',#17014,#13239,#13240);
#10613=AXIS2_PLACEMENT_3D('',#17016,#13242,#13243);
#10614=AXIS2_PLACEMENT_3D('',#17019,#13244,#13245);
#10615=AXIS2_PLACEMENT_3D('',#17020,#13246,#13247);
#10616=AXIS2_PLACEMENT_3D('',#17021,#13248,#13249);
#10617=AXIS2_PLACEMENT_3D('',#17022,#13250,#13251);
#10618=AXIS2_PLACEMENT_3D('',#17024,#13253,#13254);
#10619=AXIS2_PLACEMENT_3D('',#17026,#13255,#13256);
#10620=AXIS2_PLACEMENT_3D('',#17027,#13257,#13258);
#10621=AXIS2_PLACEMENT_3D('',#17028,#13259,#13260);
#10622=AXIS2_PLACEMENT_3D('',#17030,#13261,#13262);
#10623=AXIS2_PLACEMENT_3D('',#17032,#13263,#13264);
#10624=AXIS2_PLACEMENT_3D('',#17033,#13265,#13266);
#10625=AXIS2_PLACEMENT_3D('',#17034,#13267,#13268);
#10626=AXIS2_PLACEMENT_3D('',#17036,#13270,#13271);
#10627=AXIS2_PLACEMENT_3D('',#17038,#13272,#13273);
#10628=AXIS2_PLACEMENT_3D('',#17039,#13274,#13275);
#10629=AXIS2_PLACEMENT_3D('',#17040,#13276,#13277);
#10630=AXIS2_PLACEMENT_3D('',#17042,#13279,#13280);
#10631=AXIS2_PLACEMENT_3D('',#17045,#13281,#13282);
#10632=AXIS2_PLACEMENT_3D('',#17047,#13283,#13284);
#10633=AXIS2_PLACEMENT_3D('',#17048,#13285,#13286);
#10634=AXIS2_PLACEMENT_3D('',#17049,#13287,#13288);
#10635=AXIS2_PLACEMENT_3D('',#17052,#13291,#13292);
#10636=AXIS2_PLACEMENT_3D('',#17054,#13293,#13294);
#10637=AXIS2_PLACEMENT_3D('',#17055,#13295,#13296);
#10638=AXIS2_PLACEMENT_3D('',#17056,#13297,#13298);
#10639=AXIS2_PLACEMENT_3D('',#17059,#13299,#13300);
#10640=AXIS2_PLACEMENT_3D('',#17061,#13301,#13302);
#10641=AXIS2_PLACEMENT_3D('',#17062,#13303,#13304);
#10642=AXIS2_PLACEMENT_3D('',#17063,#13305,#13306);
#10643=AXIS2_PLACEMENT_3D('',#17066,#13309,#13310);
#10644=AXIS2_PLACEMENT_3D('',#17068,#13311,#13312);
#10645=AXIS2_PLACEMENT_3D('',#17070,#13313,#13314);
#10646=AXIS2_PLACEMENT_3D('',#17071,#13315,#13316);
#10647=AXIS2_PLACEMENT_3D('',#17072,#13317,#13318);
#10648=AXIS2_PLACEMENT_3D('',#17074,#13320,#13321);
#10649=AXIS2_PLACEMENT_3D('',#17077,#13322,#13323);
#10650=AXIS2_PLACEMENT_3D('',#17079,#13324,#13325);
#10651=AXIS2_PLACEMENT_3D('',#17080,#13326,#13327);
#10652=AXIS2_PLACEMENT_3D('',#17081,#13328,#13329);
#10653=AXIS2_PLACEMENT_3D('',#17083,#13330,#13331);
#10654=AXIS2_PLACEMENT_3D('',#17085,#13332,#13333);
#10655=AXIS2_PLACEMENT_3D('',#17086,#13334,#13335);
#10656=AXIS2_PLACEMENT_3D('',#17087,#13336,#13337);
#10657=AXIS2_PLACEMENT_3D('',#17090,#13338,#13339);
#10658=AXIS2_PLACEMENT_3D('',#17092,#13340,#13341);
#10659=AXIS2_PLACEMENT_3D('',#17093,#13342,#13343);
#10660=AXIS2_PLACEMENT_3D('',#17094,#13344,#13345);
#10661=AXIS2_PLACEMENT_3D('',#17096,#13346,#13347);
#10662=AXIS2_PLACEMENT_3D('',#17097,#13348,#13349);
#10663=AXIS2_PLACEMENT_3D('',#17098,#13350,#13351);
#10664=AXIS2_PLACEMENT_3D('',#17100,#13353,#13354);
#10665=AXIS2_PLACEMENT_3D('',#17103,#13355,#13356);
#10666=AXIS2_PLACEMENT_3D('',#17104,#13357,#13358);
#10667=AXIS2_PLACEMENT_3D('',#17105,#13359,#13360);
#10668=AXIS2_PLACEMENT_3D('',#17106,#13361,#13362);
#10669=AXIS2_PLACEMENT_3D('',#17108,#13363,#13364);
#10670=AXIS2_PLACEMENT_3D('',#17109,#13365,#13366);
#10671=AXIS2_PLACEMENT_3D('',#17110,#13367,#13368);
#10672=AXIS2_PLACEMENT_3D('',#17113,#13369,#13370);
#10673=AXIS2_PLACEMENT_3D('',#17114,#13371,#13372);
#10674=AXIS2_PLACEMENT_3D('',#17115,#13373,#13374);
#10675=AXIS2_PLACEMENT_3D('',#17116,#13375,#13376);
#10676=AXIS2_PLACEMENT_3D('',#17118,#13377,#13378);
#10677=AXIS2_PLACEMENT_3D('',#17120,#13379,#13380);
#10678=AXIS2_PLACEMENT_3D('',#17121,#13381,#13382);
#10679=AXIS2_PLACEMENT_3D('',#17122,#13383,#13384);
#10680=AXIS2_PLACEMENT_3D('',#17124,#13386,#13387);
#10681=AXIS2_PLACEMENT_3D('',#17126,#13389,#13390);
#10682=AXIS2_PLACEMENT_3D('',#17128,#13391,#13392);
#10683=AXIS2_PLACEMENT_3D('',#17130,#13393,#13394);
#10684=AXIS2_PLACEMENT_3D('',#17131,#13395,#13396);
#10685=AXIS2_PLACEMENT_3D('',#17132,#13397,#13398);
#10686=AXIS2_PLACEMENT_3D('',#17134,#13400,#13401);
#10687=AXIS2_PLACEMENT_3D('',#17136,#13403,#13404);
#10688=AXIS2_PLACEMENT_3D('',#17138,#13406,#13407);
#10689=AXIS2_PLACEMENT_3D('',#17141,#13410,#13411);
#10690=AXIS2_PLACEMENT_3D('',#17143,#13413,#13414);
#10691=AXIS2_PLACEMENT_3D('',#17145,#13416,#13417);
#10692=AXIS2_PLACEMENT_3D('',#17148,#13420,#13421);
#10693=AXIS2_PLACEMENT_3D('',#17151,#13424,#13425);
#10694=AXIS2_PLACEMENT_3D('',#17154,#13428,#13429);
#10695=AXIS2_PLACEMENT_3D('',#17156,#13431,#13432);
#10696=AXIS2_PLACEMENT_3D('',#17159,#13435,#13436);
#10697=AXIS2_PLACEMENT_3D('',#17162,#13439,#13440);
#10698=AXIS2_PLACEMENT_3D('',#17164,#13442,#13443);
#10699=AXIS2_PLACEMENT_3D('',#17166,#13445,#13446);
#10700=AXIS2_PLACEMENT_3D('',#17168,#13448,#13449);
#10701=AXIS2_PLACEMENT_3D('',#17170,#13451,#13452);
#10702=AXIS2_PLACEMENT_3D('',#17172,#13454,#13455);
#10703=AXIS2_PLACEMENT_3D('',#17174,#13457,#13458);
#10704=AXIS2_PLACEMENT_3D('',#17176,#13460,#13461);
#10705=AXIS2_PLACEMENT_3D('',#17179,#13464,#13465);
#10706=AXIS2_PLACEMENT_3D('',#17180,#13466,#13467);
#10707=AXIS2_PLACEMENT_3D('',#17181,#13468,#13469);
#10708=AXIS2_PLACEMENT_3D('',#17182,#13470,#13471);
#10709=AXIS2_PLACEMENT_3D('',#17183,#13472,#13473);
#10710=AXIS2_PLACEMENT_3D('',#17184,#13474,#13475);
#10711=AXIS2_PLACEMENT_3D('',#17185,#13476,#13477);
#10712=AXIS2_PLACEMENT_3D('',#17186,#13478,#13479);
#10713=AXIS2_PLACEMENT_3D('',#17187,#13480,#13481);
#10714=AXIS2_PLACEMENT_3D('',#17188,#13482,#13483);
#10715=AXIS2_PLACEMENT_3D('',#17189,#13484,#13485);
#10716=AXIS2_PLACEMENT_3D('',#17192,#13486,#13487);
#10717=AXIS2_PLACEMENT_3D('',#17196,#13489,#13490);
#10718=AXIS2_PLACEMENT_3D('',#17198,#13492,#13493);
#10719=AXIS2_PLACEMENT_3D('',#17201,#13494,#13495);
#10720=AXIS2_PLACEMENT_3D('',#17202,#13496,#13497);
#10721=AXIS2_PLACEMENT_3D('',#17203,#13498,#13499);
#10722=AXIS2_PLACEMENT_3D('',#17204,#13500,#13501);
#10723=AXIS2_PLACEMENT_3D('',#17207,#13502,#13503);
#10724=AXIS2_PLACEMENT_3D('',#17210,#13506,#13507);
#10725=AXIS2_PLACEMENT_3D('',#17211,#13508,#13509);
#10726=AXIS2_PLACEMENT_3D('',#17212,#13510,#13511);
#10727=AXIS2_PLACEMENT_3D('',#17213,#13512,#13513);
#10728=AXIS2_PLACEMENT_3D('',#17217,#13515,#13516);
#10729=AXIS2_PLACEMENT_3D('',#17219,#13518,#13519);
#10730=AXIS2_PLACEMENT_3D('',#17223,#13522,#13523);
#10731=AXIS2_PLACEMENT_3D('',#17232,#13528,#13529);
#10732=AXIS2_PLACEMENT_3D('',#17234,#13530,#13531);
#10733=AXIS2_PLACEMENT_3D('',#17236,#13532,#13533);
#10734=AXIS2_PLACEMENT_3D('',#17238,#13534,#13535);
#10735=AXIS2_PLACEMENT_3D('',#17239,#13536,#13537);
#10736=AXIS2_PLACEMENT_3D('',#17240,#13538,#13539);
#10737=AXIS2_PLACEMENT_3D('',#17243,#13540,#13541);
#10738=AXIS2_PLACEMENT_3D('',#17245,#13542,#13543);
#10739=AXIS2_PLACEMENT_3D('',#17246,#13544,#13545);
#10740=AXIS2_PLACEMENT_3D('',#17247,#13546,#13547);
#10741=AXIS2_PLACEMENT_3D('',#17250,#13548,#13549);
#10742=AXIS2_PLACEMENT_3D('',#17252,#13550,#13551);
#10743=AXIS2_PLACEMENT_3D('',#17253,#13552,#13553);
#10744=AXIS2_PLACEMENT_3D('',#17254,#13554,#13555);
#10745=AXIS2_PLACEMENT_3D('',#17255,#13556,#13557);
#10746=AXIS2_PLACEMENT_3D('',#17260,#13560,#13561);
#10747=AXIS2_PLACEMENT_3D('',#17261,#13562,#13563);
#10748=AXIS2_PLACEMENT_3D('',#17264,#13564,#13565);
#10749=AXIS2_PLACEMENT_3D('',#17265,#13566,#13567);
#10750=AXIS2_PLACEMENT_3D('',#17266,#13568,#13569);
#10751=AXIS2_PLACEMENT_3D('',#17267,#13570,#13571);
#10752=AXIS2_PLACEMENT_3D('',#17270,#13572,#13573);
#10753=AXIS2_PLACEMENT_3D('',#17272,#13574,#13575);
#10754=AXIS2_PLACEMENT_3D('',#17273,#13576,#13577);
#10755=AXIS2_PLACEMENT_3D('',#17274,#13578,#13579);
#10756=AXIS2_PLACEMENT_3D('',#17277,#13582,#13583);
#10757=AXIS2_PLACEMENT_3D('',#17280,#13584,#13585);
#10758=AXIS2_PLACEMENT_3D('',#17282,#13586,#13587);
#10759=AXIS2_PLACEMENT_3D('',#17283,#13588,#13589);
#10760=AXIS2_PLACEMENT_3D('',#17284,#13590,#13591);
#10761=AXIS2_PLACEMENT_3D('',#17286,#13592,#13593);
#10762=AXIS2_PLACEMENT_3D('',#17288,#13594,#13595);
#10763=AXIS2_PLACEMENT_3D('',#17289,#13596,#13597);
#10764=AXIS2_PLACEMENT_3D('',#17290,#13598,#13599);
#10765=AXIS2_PLACEMENT_3D('',#17293,#13600,#13601);
#10766=AXIS2_PLACEMENT_3D('',#17295,#13602,#13603);
#10767=AXIS2_PLACEMENT_3D('',#17296,#13604,#13605);
#10768=AXIS2_PLACEMENT_3D('',#17297,#13606,#13607);
#10769=AXIS2_PLACEMENT_3D('',#17300,#13608,#13609);
#10770=AXIS2_PLACEMENT_3D('',#17302,#13610,#13611);
#10771=AXIS2_PLACEMENT_3D('',#17303,#13612,#13613);
#10772=AXIS2_PLACEMENT_3D('',#17304,#13614,#13615);
#10773=AXIS2_PLACEMENT_3D('',#17307,#13618,#13619);
#10774=AXIS2_PLACEMENT_3D('',#17310,#13620,#13621);
#10775=AXIS2_PLACEMENT_3D('',#17312,#13622,#13623);
#10776=AXIS2_PLACEMENT_3D('',#17313,#13624,#13625);
#10777=AXIS2_PLACEMENT_3D('',#17314,#13626,#13627);
#10778=AXIS2_PLACEMENT_3D('',#17317,#13630,#13631);
#10779=AXIS2_PLACEMENT_3D('',#17320,#13634,#13635);
#10780=AXIS2_PLACEMENT_3D('',#17323,#13638,#13639);
#10781=AXIS2_PLACEMENT_3D('',#17326,#13642,#13643);
#10782=AXIS2_PLACEMENT_3D('',#17329,#13646,#13647);
#10783=AXIS2_PLACEMENT_3D('',#17332,#13650,#13651);
#10784=AXIS2_PLACEMENT_3D('',#17334,#13653,#13654);
#10785=AXIS2_PLACEMENT_3D('',#17336,#13656,#13657);
#10786=AXIS2_PLACEMENT_3D('',#17339,#13660,#13661);
#10787=AXIS2_PLACEMENT_3D('',#17342,#13664,#13665);
#10788=AXIS2_PLACEMENT_3D('',#17344,#13667,#13668);
#10789=AXIS2_PLACEMENT_3D('',#17346,#13670,#13671);
#10790=AXIS2_PLACEMENT_3D('',#17351,#13674,#13675);
#10791=AXIS2_PLACEMENT_3D('',#17352,#13676,#13677);
#10792=AXIS2_PLACEMENT_3D('',#17355,#13680,#13681);
#10793=AXIS2_PLACEMENT_3D('',#17357,#13683,#13684);
#10794=AXIS2_PLACEMENT_3D('',#17358,#13685,#13686);
#10795=AXIS2_PLACEMENT_3D('',#17359,#13687,#13688);
#10796=AXIS2_PLACEMENT_3D('',#17364,#13690,#13691);
#10797=AXIS2_PLACEMENT_3D('',#17367,#13693,#13694);
#10798=AXIS2_PLACEMENT_3D('',#17368,#13695,#13696);
#10799=AXIS2_PLACEMENT_3D('',#17369,#13697,#13698);
#10800=AXIS2_PLACEMENT_3D('',#17370,#13699,#13700);
#10801=AXIS2_PLACEMENT_3D('',#17371,#13701,#13702);
#10802=AXIS2_PLACEMENT_3D('',#17372,#13703,#13704);
#10803=AXIS2_PLACEMENT_3D('',#17373,#13705,#13706);
#10804=AXIS2_PLACEMENT_3D('',#17375,#13707,#13708);
#10805=AXIS2_PLACEMENT_3D('',#17376,#13709,#13710);
#10806=AXIS2_PLACEMENT_3D('',#17377,#13711,#13712);
#10807=AXIS2_PLACEMENT_3D('',#17378,#13713,#13714);
#10808=AXIS2_PLACEMENT_3D('',#17380,#13716,#13717);
#10809=AXIS2_PLACEMENT_3D('',#17381,#13718,#13719);
#10810=AXIS2_PLACEMENT_3D('',#17383,#13721,#13722);
#10811=AXIS2_PLACEMENT_3D('',#17384,#13723,#13724);
#10812=AXIS2_PLACEMENT_3D('',#17385,#13725,#13726);
#10813=AXIS2_PLACEMENT_3D('',#17386,#13727,#13728);
#10814=AXIS2_PLACEMENT_3D('',#17388,#13729,#13730);
#10815=AXIS2_PLACEMENT_3D('',#17390,#13731,#13732);
#10816=AXIS2_PLACEMENT_3D('',#17391,#13733,#13734);
#10817=AXIS2_PLACEMENT_3D('',#17393,#13735,#13736);
#10818=AXIS2_PLACEMENT_3D('',#17396,#13738,#13739);
#10819=AXIS2_PLACEMENT_3D('',#17397,#13740,#13741);
#10820=AXIS2_PLACEMENT_3D('',#17400,#13743,#13744);
#10821=AXIS2_PLACEMENT_3D('',#17401,#13745,#13746);
#10822=AXIS2_PLACEMENT_3D('',#17402,#13747,#13748);
#10823=AXIS2_PLACEMENT_3D('',#17404,#13750,#13751);
#10824=AXIS2_PLACEMENT_3D('',#17407,#13753,#13754);
#10825=AXIS2_PLACEMENT_3D('',#17408,#13755,#13756);
#10826=AXIS2_PLACEMENT_3D('',#17409,#13757,#13758);
#10827=AXIS2_PLACEMENT_3D('',#17410,#13759,#13760);
#10828=AXIS2_PLACEMENT_3D('',#17413,#13761,#13762);
#10829=AXIS2_PLACEMENT_3D('',#17417,#13764,#13765);
#10830=AXIS2_PLACEMENT_3D('',#17419,#13767,#13768);
#10831=AXIS2_PLACEMENT_3D('',#17422,#13769,#13770);
#10832=AXIS2_PLACEMENT_3D('',#17423,#13771,#13772);
#10833=AXIS2_PLACEMENT_3D('',#17424,#13773,#13774);
#10834=AXIS2_PLACEMENT_3D('',#17425,#13775,#13776);
#10835=AXIS2_PLACEMENT_3D('',#17428,#13777,#13778);
#10836=AXIS2_PLACEMENT_3D('',#17431,#13781,#13782);
#10837=AXIS2_PLACEMENT_3D('',#17432,#13783,#13784);
#10838=AXIS2_PLACEMENT_3D('',#17433,#13785,#13786);
#10839=AXIS2_PLACEMENT_3D('',#17434,#13787,#13788);
#10840=AXIS2_PLACEMENT_3D('',#17438,#13790,#13791);
#10841=AXIS2_PLACEMENT_3D('',#17440,#13793,#13794);
#10842=AXIS2_PLACEMENT_3D('',#17444,#13797,#13798);
#10843=AXIS2_PLACEMENT_3D('',#17453,#13803,#13804);
#10844=AXIS2_PLACEMENT_3D('',#17455,#13805,#13806);
#10845=AXIS2_PLACEMENT_3D('',#17457,#13807,#13808);
#10846=AXIS2_PLACEMENT_3D('',#17459,#13809,#13810);
#10847=AXIS2_PLACEMENT_3D('',#17460,#13811,#13812);
#10848=AXIS2_PLACEMENT_3D('',#17461,#13813,#13814);
#10849=AXIS2_PLACEMENT_3D('',#17464,#13815,#13816);
#10850=AXIS2_PLACEMENT_3D('',#17466,#13817,#13818);
#10851=AXIS2_PLACEMENT_3D('',#17467,#13819,#13820);
#10852=AXIS2_PLACEMENT_3D('',#17468,#13821,#13822);
#10853=AXIS2_PLACEMENT_3D('',#17471,#13823,#13824);
#10854=AXIS2_PLACEMENT_3D('',#17472,#13825,#13826);
#10855=AXIS2_PLACEMENT_3D('',#17474,#13827,#13828);
#10856=AXIS2_PLACEMENT_3D('',#17475,#13829,#13830);
#10857=AXIS2_PLACEMENT_3D('',#17476,#13831,#13832);
#10858=AXIS2_PLACEMENT_3D('',#17480,#13834,#13835);
#10859=AXIS2_PLACEMENT_3D('',#17482,#13837,#13838);
#10860=AXIS2_PLACEMENT_3D('',#17485,#13839,#13840);
#10861=AXIS2_PLACEMENT_3D('',#17486,#13841,#13842);
#10862=AXIS2_PLACEMENT_3D('',#17487,#13843,#13844);
#10863=AXIS2_PLACEMENT_3D('',#17488,#13845,#13846);
#10864=AXIS2_PLACEMENT_3D('',#17491,#13847,#13848);
#10865=AXIS2_PLACEMENT_3D('',#17493,#13849,#13850);
#10866=AXIS2_PLACEMENT_3D('',#17494,#13851,#13852);
#10867=AXIS2_PLACEMENT_3D('',#17495,#13853,#13854);
#10868=AXIS2_PLACEMENT_3D('',#17498,#13857,#13858);
#10869=AXIS2_PLACEMENT_3D('',#17501,#13859,#13860);
#10870=AXIS2_PLACEMENT_3D('',#17503,#13861,#13862);
#10871=AXIS2_PLACEMENT_3D('',#17504,#13863,#13864);
#10872=AXIS2_PLACEMENT_3D('',#17505,#13865,#13866);
#10873=AXIS2_PLACEMENT_3D('',#17507,#13867,#13868);
#10874=AXIS2_PLACEMENT_3D('',#17509,#13869,#13870);
#10875=AXIS2_PLACEMENT_3D('',#17510,#13871,#13872);
#10876=AXIS2_PLACEMENT_3D('',#17511,#13873,#13874);
#10877=AXIS2_PLACEMENT_3D('',#17514,#13875,#13876);
#10878=AXIS2_PLACEMENT_3D('',#17516,#13877,#13878);
#10879=AXIS2_PLACEMENT_3D('',#17517,#13879,#13880);
#10880=AXIS2_PLACEMENT_3D('',#17518,#13881,#13882);
#10881=AXIS2_PLACEMENT_3D('',#17521,#13883,#13884);
#10882=AXIS2_PLACEMENT_3D('',#17523,#13885,#13886);
#10883=AXIS2_PLACEMENT_3D('',#17524,#13887,#13888);
#10884=AXIS2_PLACEMENT_3D('',#17525,#13889,#13890);
#10885=AXIS2_PLACEMENT_3D('',#17528,#13893,#13894);
#10886=AXIS2_PLACEMENT_3D('',#17531,#13895,#13896);
#10887=AXIS2_PLACEMENT_3D('',#17533,#13897,#13898);
#10888=AXIS2_PLACEMENT_3D('',#17534,#13899,#13900);
#10889=AXIS2_PLACEMENT_3D('',#17535,#13901,#13902);
#10890=AXIS2_PLACEMENT_3D('',#17538,#13905,#13906);
#10891=AXIS2_PLACEMENT_3D('',#17541,#13909,#13910);
#10892=AXIS2_PLACEMENT_3D('',#17544,#13913,#13914);
#10893=AXIS2_PLACEMENT_3D('',#17547,#13917,#13918);
#10894=AXIS2_PLACEMENT_3D('',#17550,#13921,#13922);
#10895=AXIS2_PLACEMENT_3D('',#17553,#13925,#13926);
#10896=AXIS2_PLACEMENT_3D('',#17555,#13928,#13929);
#10897=AXIS2_PLACEMENT_3D('',#17557,#13931,#13932);
#10898=AXIS2_PLACEMENT_3D('',#17560,#13935,#13936);
#10899=AXIS2_PLACEMENT_3D('',#17563,#13939,#13940);
#10900=AXIS2_PLACEMENT_3D('',#17565,#13942,#13943);
#10901=AXIS2_PLACEMENT_3D('',#17567,#13945,#13946);
#10902=AXIS2_PLACEMENT_3D('',#17571,#13948,#13949);
#10903=AXIS2_PLACEMENT_3D('',#17573,#13951,#13952);
#10904=AXIS2_PLACEMENT_3D('',#17576,#13955,#13956);
#10905=AXIS2_PLACEMENT_3D('',#17578,#13958,#13959);
#10906=AXIS2_PLACEMENT_3D('',#17579,#13960,#13961);
#10907=AXIS2_PLACEMENT_3D('',#17580,#13962,#13963);
#10908=AXIS2_PLACEMENT_3D('',#17585,#13965,#13966);
#10909=AXIS2_PLACEMENT_3D('',#17588,#13968,#13969);
#10910=AXIS2_PLACEMENT_3D('',#17589,#13970,#13971);
#10911=AXIS2_PLACEMENT_3D('',#17590,#13972,#13973);
#10912=AXIS2_PLACEMENT_3D('',#17591,#13974,#13975);
#10913=AXIS2_PLACEMENT_3D('',#17592,#13976,#13977);
#10914=AXIS2_PLACEMENT_3D('',#17593,#13978,#13979);
#10915=AXIS2_PLACEMENT_3D('',#17594,#13980,#13981);
#10916=AXIS2_PLACEMENT_3D('',#17596,#13982,#13983);
#10917=AXIS2_PLACEMENT_3D('',#17597,#13984,#13985);
#10918=AXIS2_PLACEMENT_3D('',#17598,#13986,#13987);
#10919=AXIS2_PLACEMENT_3D('',#17599,#13988,#13989);
#10920=AXIS2_PLACEMENT_3D('',#17601,#13991,#13992);
#10921=AXIS2_PLACEMENT_3D('',#17602,#13993,#13994);
#10922=AXIS2_PLACEMENT_3D('',#17604,#13996,#13997);
#10923=AXIS2_PLACEMENT_3D('',#17605,#13998,#13999);
#10924=AXIS2_PLACEMENT_3D('',#17606,#14000,#14001);
#10925=AXIS2_PLACEMENT_3D('',#17607,#14002,#14003);
#10926=AXIS2_PLACEMENT_3D('',#17610,#14004,#14005);
#10927=AXIS2_PLACEMENT_3D('',#17614,#14007,#14008);
#10928=AXIS2_PLACEMENT_3D('',#17616,#14010,#14011);
#10929=AXIS2_PLACEMENT_3D('',#17619,#14012,#14013);
#10930=AXIS2_PLACEMENT_3D('',#17620,#14014,#14015);
#10931=AXIS2_PLACEMENT_3D('',#17621,#14016,#14017);
#10932=AXIS2_PLACEMENT_3D('',#17622,#14018,#14019);
#10933=AXIS2_PLACEMENT_3D('',#17625,#14020,#14021);
#10934=AXIS2_PLACEMENT_3D('',#17628,#14024,#14025);
#10935=AXIS2_PLACEMENT_3D('',#17629,#14026,#14027);
#10936=AXIS2_PLACEMENT_3D('',#17630,#14028,#14029);
#10937=AXIS2_PLACEMENT_3D('',#17631,#14030,#14031);
#10938=AXIS2_PLACEMENT_3D('',#17635,#14033,#14034);
#10939=AXIS2_PLACEMENT_3D('',#17637,#14036,#14037);
#10940=AXIS2_PLACEMENT_3D('',#17641,#14040,#14041);
#10941=AXIS2_PLACEMENT_3D('',#17650,#14046,#14047);
#10942=AXIS2_PLACEMENT_3D('',#17652,#14048,#14049);
#10943=AXIS2_PLACEMENT_3D('',#17654,#14050,#14051);
#10944=AXIS2_PLACEMENT_3D('',#17656,#14052,#14053);
#10945=AXIS2_PLACEMENT_3D('',#17657,#14054,#14055);
#10946=AXIS2_PLACEMENT_3D('',#17658,#14056,#14057);
#10947=AXIS2_PLACEMENT_3D('',#17661,#14058,#14059);
#10948=AXIS2_PLACEMENT_3D('',#17663,#14060,#14061);
#10949=AXIS2_PLACEMENT_3D('',#17664,#14062,#14063);
#10950=AXIS2_PLACEMENT_3D('',#17665,#14064,#14065);
#10951=AXIS2_PLACEMENT_3D('',#17668,#14066,#14067);
#10952=AXIS2_PLACEMENT_3D('',#17670,#14068,#14069);
#10953=AXIS2_PLACEMENT_3D('',#17671,#14070,#14071);
#10954=AXIS2_PLACEMENT_3D('',#17672,#14072,#14073);
#10955=AXIS2_PLACEMENT_3D('',#17673,#14074,#14075);
#10956=AXIS2_PLACEMENT_3D('',#17678,#14078,#14079);
#10957=AXIS2_PLACEMENT_3D('',#17679,#14080,#14081);
#10958=AXIS2_PLACEMENT_3D('',#17682,#14082,#14083);
#10959=AXIS2_PLACEMENT_3D('',#17683,#14084,#14085);
#10960=AXIS2_PLACEMENT_3D('',#17684,#14086,#14087);
#10961=AXIS2_PLACEMENT_3D('',#17685,#14088,#14089);
#10962=AXIS2_PLACEMENT_3D('',#17688,#14090,#14091);
#10963=AXIS2_PLACEMENT_3D('',#17690,#14092,#14093);
#10964=AXIS2_PLACEMENT_3D('',#17691,#14094,#14095);
#10965=AXIS2_PLACEMENT_3D('',#17692,#14096,#14097);
#10966=AXIS2_PLACEMENT_3D('',#17695,#14100,#14101);
#10967=AXIS2_PLACEMENT_3D('',#17698,#14102,#14103);
#10968=AXIS2_PLACEMENT_3D('',#17700,#14104,#14105);
#10969=AXIS2_PLACEMENT_3D('',#17701,#14106,#14107);
#10970=AXIS2_PLACEMENT_3D('',#17702,#14108,#14109);
#10971=AXIS2_PLACEMENT_3D('',#17704,#14110,#14111);
#10972=AXIS2_PLACEMENT_3D('',#17706,#14112,#14113);
#10973=AXIS2_PLACEMENT_3D('',#17707,#14114,#14115);
#10974=AXIS2_PLACEMENT_3D('',#17708,#14116,#14117);
#10975=AXIS2_PLACEMENT_3D('',#17711,#14118,#14119);
#10976=AXIS2_PLACEMENT_3D('',#17713,#14120,#14121);
#10977=AXIS2_PLACEMENT_3D('',#17714,#14122,#14123);
#10978=AXIS2_PLACEMENT_3D('',#17715,#14124,#14125);
#10979=AXIS2_PLACEMENT_3D('',#17718,#14126,#14127);
#10980=AXIS2_PLACEMENT_3D('',#17720,#14128,#14129);
#10981=AXIS2_PLACEMENT_3D('',#17721,#14130,#14131);
#10982=AXIS2_PLACEMENT_3D('',#17722,#14132,#14133);
#10983=AXIS2_PLACEMENT_3D('',#17725,#14136,#14137);
#10984=AXIS2_PLACEMENT_3D('',#17728,#14138,#14139);
#10985=AXIS2_PLACEMENT_3D('',#17730,#14140,#14141);
#10986=AXIS2_PLACEMENT_3D('',#17731,#14142,#14143);
#10987=AXIS2_PLACEMENT_3D('',#17732,#14144,#14145);
#10988=AXIS2_PLACEMENT_3D('',#17735,#14148,#14149);
#10989=AXIS2_PLACEMENT_3D('',#17738,#14152,#14153);
#10990=AXIS2_PLACEMENT_3D('',#17741,#14156,#14157);
#10991=AXIS2_PLACEMENT_3D('',#17744,#14160,#14161);
#10992=AXIS2_PLACEMENT_3D('',#17747,#14164,#14165);
#10993=AXIS2_PLACEMENT_3D('',#17750,#14168,#14169);
#10994=AXIS2_PLACEMENT_3D('',#17752,#14171,#14172);
#10995=AXIS2_PLACEMENT_3D('',#17754,#14174,#14175);
#10996=AXIS2_PLACEMENT_3D('',#17757,#14178,#14179);
#10997=AXIS2_PLACEMENT_3D('',#17760,#14182,#14183);
#10998=AXIS2_PLACEMENT_3D('',#17762,#14185,#14186);
#10999=AXIS2_PLACEMENT_3D('',#17764,#14188,#14189);
#11000=AXIS2_PLACEMENT_3D('',#17769,#14192,#14193);
#11001=AXIS2_PLACEMENT_3D('',#17770,#14194,#14195);
#11002=AXIS2_PLACEMENT_3D('',#17773,#14198,#14199);
#11003=AXIS2_PLACEMENT_3D('',#17775,#14201,#14202);
#11004=AXIS2_PLACEMENT_3D('',#17776,#14203,#14204);
#11005=AXIS2_PLACEMENT_3D('',#17777,#14205,#14206);
#11006=AXIS2_PLACEMENT_3D('',#17782,#14208,#14209);
#11007=AXIS2_PLACEMENT_3D('',#17785,#14211,#14212);
#11008=AXIS2_PLACEMENT_3D('',#17786,#14213,#14214);
#11009=AXIS2_PLACEMENT_3D('',#17787,#14215,#14216);
#11010=AXIS2_PLACEMENT_3D('',#17788,#14217,#14218);
#11011=AXIS2_PLACEMENT_3D('',#17789,#14219,#14220);
#11012=AXIS2_PLACEMENT_3D('',#17790,#14221,#14222);
#11013=AXIS2_PLACEMENT_3D('',#17791,#14223,#14224);
#11014=AXIS2_PLACEMENT_3D('',#17793,#14225,#14226);
#11015=AXIS2_PLACEMENT_3D('',#17794,#14227,#14228);
#11016=AXIS2_PLACEMENT_3D('',#17795,#14229,#14230);
#11017=AXIS2_PLACEMENT_3D('',#17796,#14231,#14232);
#11018=AXIS2_PLACEMENT_3D('',#17798,#14234,#14235);
#11019=AXIS2_PLACEMENT_3D('',#17799,#14236,#14237);
#11020=AXIS2_PLACEMENT_3D('',#17801,#14239,#14240);
#11021=AXIS2_PLACEMENT_3D('',#17802,#14241,#14242);
#11022=AXIS2_PLACEMENT_3D('',#17803,#14243,#14244);
#11023=AXIS2_PLACEMENT_3D('',#17804,#14245,#14246);
#11024=AXIS2_PLACEMENT_3D('',#17805,#14247,#14248);
#11025=AXIS2_PLACEMENT_3D('',#17806,#14249,#14250);
#11026=AXIS2_PLACEMENT_3D('',#17807,#14251,#14252);
#11027=AXIS2_PLACEMENT_3D('',#17808,#14253,#14254);
#11028=AXIS2_PLACEMENT_3D('',#17809,#14255,#14256);
#11029=AXIS2_PLACEMENT_3D('',#17810,#14257,#14258);
#11030=AXIS2_PLACEMENT_3D('',#17811,#14259,#14260);
#11031=AXIS2_PLACEMENT_3D('',#17812,#14261,#14262);
#11032=DIRECTION('axis',(0.,0.,1.));
#11033=DIRECTION('refdir',(1.,0.,0.));
#11034=DIRECTION('axis',(0.,0.,1.));
#11035=DIRECTION('refdir',(1.,0.,0.));
#11036=DIRECTION('center_axis',(0.,-1.,0.));
#11037=DIRECTION('ref_axis',(1.,0.,0.));
#11038=DIRECTION('center_axis',(0.,-1.,0.));
#11039=DIRECTION('ref_axis',(1.,0.,0.));
#11040=DIRECTION('center_axis',(0.,-1.,0.));
#11041=DIRECTION('ref_axis',(1.,0.,0.));
#11042=DIRECTION('center_axis',(0.,1.,0.));
#11043=DIRECTION('ref_axis',(1.,0.,0.));
#11044=DIRECTION('center_axis',(0.,1.,0.));
#11045=DIRECTION('ref_axis',(1.,0.,0.));
#11046=DIRECTION('',(-0.707106781186549,0.707106781186546,-8.65956056235495E-17));
#11047=DIRECTION('center_axis',(0.,-1.,0.));
#11048=DIRECTION('ref_axis',(1.,0.,0.));
#11049=DIRECTION('center_axis',(0.,-1.,0.));
#11050=DIRECTION('ref_axis',(1.,0.,0.));
#11051=DIRECTION('',(0.,1.,0.));
#11052=DIRECTION('center_axis',(0.,1.,0.));
#11053=DIRECTION('ref_axis',(1.,0.,0.));
#11054=DIRECTION('center_axis',(0.,-1.,0.));
#11055=DIRECTION('ref_axis',(1.,0.,0.));
#11056=DIRECTION('center_axis',(0.,-1.,0.));
#11057=DIRECTION('ref_axis',(1.,0.,0.));
#11058=DIRECTION('',(0.707106781186549,0.707106781186546,8.65956056235495E-17));
#11059=DIRECTION('center_axis',(0.,-1.,0.));
#11060=DIRECTION('ref_axis',(1.,0.,0.));
#11061=DIRECTION('',(0.,1.,0.));
#11062=DIRECTION('center_axis',(0.,-1.,0.));
#11063=DIRECTION('ref_axis',(1.,0.,0.));
#11064=DIRECTION('center_axis',(0.,-1.,0.));
#11065=DIRECTION('ref_axis',(1.,0.,0.));
#11066=DIRECTION('axis',(0.,0.,1.));
#11067=DIRECTION('refdir',(1.,0.,0.));
#11068=DIRECTION('center_axis',(0.,0.,-1.));
#11069=DIRECTION('ref_axis',(-1.,0.,0.));
#11070=DIRECTION('center_axis',(0.,0.,1.));
#11071=DIRECTION('ref_axis',(0.707106781186548,-0.707106781186548,0.));
#11072=DIRECTION('',(1.,0.,0.));
#11073=DIRECTION('',(0.,1.,0.));
#11074=DIRECTION('',(-1.,0.,0.));
#11075=DIRECTION('center_axis',(0.,0.,1.));
#11076=DIRECTION('ref_axis',(0.707106781186548,0.707106781186548,0.));
#11077=DIRECTION('',(0.,1.,0.));
#11078=DIRECTION('center_axis',(0.,0.,1.));
#11079=DIRECTION('ref_axis',(1.,0.,0.));
#11080=DIRECTION('center_axis',(0.,0.,-1.));
#11081=DIRECTION('ref_axis',(0.707106781186548,-0.707106781186548,0.));
#11082=DIRECTION('',(0.,-1.,0.));
#11083=DIRECTION('center_axis',(0.,0.,-1.));
#11084=DIRECTION('ref_axis',(0.707106781186548,0.707106781186548,0.));
#11085=DIRECTION('',(1.,0.,0.));
#11086=DIRECTION('',(0.,1.,0.));
#11087=DIRECTION('',(-1.,0.,0.));
#11088=DIRECTION('center_axis',(1.,0.,0.));
#11089=DIRECTION('ref_axis',(0.,0.,-1.));
#11090=DIRECTION('',(0.,0.,-1.));
#11091=DIRECTION('',(0.,0.,1.));
#11092=DIRECTION('center_axis',(0.,0.,1.));
#11093=DIRECTION('ref_axis',(0.707106781186548,-0.707106781186548,0.));
#11094=DIRECTION('',(0.,0.,-1.));
#11095=DIRECTION('center_axis',(0.707106781186543,0.,0.707106781186553));
#11096=DIRECTION('ref_axis',(0.707106781186553,0.,-0.707106781186543));
#11097=DIRECTION('',(0.,0.,1.));
#11098=DIRECTION('center_axis',(0.,0.,1.));
#11099=DIRECTION('ref_axis',(0.707106781186548,-0.707106781186548,0.));
#11100=DIRECTION('',(0.,0.,1.));
#11101=DIRECTION('center_axis',(0.,0.,1.));
#11102=DIRECTION('ref_axis',(1.,0.,0.));
#11103=DIRECTION('',(0.,0.,-1.));
#11104=DIRECTION('center_axis',(1.,0.,0.));
#11105=DIRECTION('ref_axis',(0.,1.,0.));
#11106=DIRECTION('',(0.,1.,0.));
#11107=DIRECTION('',(0.,0.,-1.));
#11108=DIRECTION('center_axis',(1.,0.,0.));
#11109=DIRECTION('ref_axis',(0.,1.,0.));
#11110=DIRECTION('',(0.,0.,-1.));
#11111=DIRECTION('',(0.,1.,0.));
#11112=DIRECTION('center_axis',(0.,0.,1.));
#11113=DIRECTION('ref_axis',(0.707106781186548,0.707106781186548,0.));
#11114=DIRECTION('center_axis',(-0.707106781186543,0.,-0.707106781186553));
#11115=DIRECTION('ref_axis',(0.707106781186553,0.,-0.707106781186542));
#11116=DIRECTION('',(0.,0.,1.));
#11117=DIRECTION('center_axis',(0.,0.,1.));
#11118=DIRECTION('ref_axis',(0.707106781186548,0.707106781186548,0.));
#11119=DIRECTION('',(0.,0.,1.));
#11120=DIRECTION('center_axis',(0.,0.,1.));
#11121=DIRECTION('ref_axis',(0.,1.,0.));
#11122=DIRECTION('center_axis',(0.,1.,0.));
#11123=DIRECTION('ref_axis',(-1.,0.,0.));
#11124=DIRECTION('',(1.,0.,0.));
#11125=DIRECTION('',(0.,0.,-1.));
#11126=DIRECTION('',(1.,0.,0.));
#11127=DIRECTION('',(0.,0.,1.));
#11128=DIRECTION('',(-1.,0.,0.));
#11129=DIRECTION('',(0.,0.,-1.));
#11130=DIRECTION('',(-1.,0.,0.));
#11131=DIRECTION('',(0.707106781186548,0.,0.707106781186548));
#11132=DIRECTION('center_axis',(0.,1.,0.));
#11133=DIRECTION('ref_axis',(-0.923879532511307,0.,-0.38268343236504));
#11134=DIRECTION('',(-1.,0.,0.));
#11135=DIRECTION('',(0.,0.,1.));
#11136=DIRECTION('center_axis',(0.,1.,0.));
#11137=DIRECTION('ref_axis',(-0.70710678118655,0.,-0.707106781186544));
#11138=DIRECTION('',(-1.,0.,0.));
#11139=DIRECTION('center_axis',(0.,1.,0.));
#11140=DIRECTION('ref_axis',(0.707106781186546,0.,-0.707106781186549));
#11141=DIRECTION('',(0.,0.,-1.));
#11142=DIRECTION('',(-1.,0.,0.));
#11143=DIRECTION('center_axis',(0.,1.,0.));
#11144=DIRECTION('ref_axis',(0.707106781186546,0.,-0.707106781186549));
#11145=DIRECTION('',(0.,0.,-1.));
#11146=DIRECTION('',(-1.,0.,0.));
#11147=DIRECTION('center_axis',(0.,0.,1.));
#11148=DIRECTION('ref_axis',(1.,0.,0.));
#11149=DIRECTION('center_axis',(0.,0.,1.));
#11150=DIRECTION('ref_axis',(-0.707106781186548,0.707106781186548,0.));
#11151=DIRECTION('',(0.,1.,0.));
#11152=DIRECTION('',(1.,0.,0.));
#11153=DIRECTION('center_axis',(0.,0.,1.));
#11154=DIRECTION('ref_axis',(-0.707106781186548,-0.707106781186548,0.));
#11155=DIRECTION('',(0.,-1.,0.));
#11156=DIRECTION('center_axis',(0.,0.,-1.));
#11157=DIRECTION('ref_axis',(-1.,0.,0.));
#11158=DIRECTION('center_axis',(0.,0.,-1.));
#11159=DIRECTION('ref_axis',(-0.707106781186548,0.707106781186548,0.));
#11160=DIRECTION('',(0.,1.,0.));
#11161=DIRECTION('center_axis',(0.,0.,-1.));
#11162=DIRECTION('ref_axis',(-0.707106781186548,-0.707106781186548,0.));
#11163=DIRECTION('',(-1.,0.,0.));
#11164=DIRECTION('',(0.,1.,0.));
#11165=DIRECTION('center_axis',(1.,0.,0.));
#11166=DIRECTION('ref_axis',(0.,0.,-1.));
#11167=DIRECTION('',(0.,0.,-1.));
#11168=DIRECTION('center_axis',(0.,0.,1.));
#11169=DIRECTION('ref_axis',(-0.707106781186548,0.707106781186548,0.));
#11170=DIRECTION('',(0.,0.,1.));
#11171=DIRECTION('center_axis',(0.,0.,1.));
#11172=DIRECTION('ref_axis',(-1.,0.,0.));
#11173=DIRECTION('center_axis',(0.,-1.,0.));
#11174=DIRECTION('ref_axis',(1.,0.,0.));
#11175=DIRECTION('',(1.,0.,0.));
#11176=DIRECTION('',(0.,0.,1.));
#11177=DIRECTION('center_axis',(0.,-1.,0.));
#11178=DIRECTION('ref_axis',(0.707106781186552,0.,-0.707106781186543));
#11179=DIRECTION('',(1.,0.,0.));
#11180=DIRECTION('',(0.,0.,1.));
#11181=DIRECTION('center_axis',(0.,-1.,0.));
#11182=DIRECTION('ref_axis',(0.707106781186546,0.,-0.707106781186549));
#11183=DIRECTION('',(1.,0.,0.));
#11184=DIRECTION('center_axis',(0.,-1.,0.));
#11185=DIRECTION('ref_axis',(-0.707106781186547,0.,-0.707106781186547));
#11186=DIRECTION('',(0.,0.,-1.));
#11187=DIRECTION('',(1.,0.,0.));
#11188=DIRECTION('center_axis',(0.,-1.,0.));
#11189=DIRECTION('ref_axis',(-0.923879532511279,0.,-0.382683432365108));
#11190=DIRECTION('',(-0.707106781186548,0.,-0.707106781186548));
#11191=DIRECTION('',(1.,0.,0.));
#11192=DIRECTION('',(0.,0.,1.));
#11193=DIRECTION('',(0.,0.,1.));
#11194=DIRECTION('',(-1.,0.,0.));
#11195=DIRECTION('center_axis',(-1.,0.,0.));
#11196=DIRECTION('ref_axis',(0.,-1.,0.));
#11197=DIRECTION('',(0.,0.,-1.));
#11198=DIRECTION('',(0.,-1.,0.));
#11199=DIRECTION('center_axis',(0.,0.,1.));
#11200=DIRECTION('ref_axis',(-0.707106781186548,-0.707106781186548,0.));
#11201=DIRECTION('',(0.,0.,-1.));
#11202=DIRECTION('center_axis',(0.,0.,-1.));
#11203=DIRECTION('ref_axis',(-1.,0.,0.));
#11204=DIRECTION('center_axis',(0.,1.,0.));
#11205=DIRECTION('ref_axis',(0.,0.,1.));
#11206=DIRECTION('center_axis',(-1.,0.,0.));
#11207=DIRECTION('ref_axis',(0.,0.,1.));
#11208=DIRECTION('center_axis',(0.,-1.,0.));
#11209=DIRECTION('ref_axis',(1.,0.,0.));
#11210=DIRECTION('center_axis',(0.,0.,1.));
#11211=DIRECTION('ref_axis',(0.,1.,0.));
#11212=DIRECTION('center_axis',(0.,-1.,0.));
#11213=DIRECTION('ref_axis',(0.,0.,-1.));
#11214=DIRECTION('center_axis',(0.,0.,1.));
#11215=DIRECTION('ref_axis',(-1.,0.,0.));
#11216=DIRECTION('center_axis',(0.,1.,0.));
#11217=DIRECTION('ref_axis',(0.,0.,-1.));
#11218=DIRECTION('center_axis',(-1.,0.,0.));
#11219=DIRECTION('ref_axis',(0.,-1.,0.));
#11220=DIRECTION('center_axis',(-0.81649658092773,-0.408248290463861,-0.408248290463858));
#11221=DIRECTION('ref_axis',(-0.577350269189626,0.577350269189626,0.577350269189626));
#11222=DIRECTION('center_axis',(-1.,0.,0.));
#11223=DIRECTION('ref_axis',(0.,1.,0.));
#11224=DIRECTION('center_axis',(0.,0.,1.));
#11225=DIRECTION('ref_axis',(-1.,0.,0.));
#11226=DIRECTION('center_axis',(0.,1.,0.));
#11227=DIRECTION('ref_axis',(0.,0.,1.));
#11228=DIRECTION('center_axis',(-0.816496580927728,-0.408248290463864,-0.408248290463857));
#11229=DIRECTION('ref_axis',(-0.577350269189628,0.577350269189628,0.577350269189621));
#11230=DIRECTION('center_axis',(-1.,0.,0.));
#11231=DIRECTION('ref_axis',(0.,1.,0.));
#11232=DIRECTION('center_axis',(0.,4.44089209850056E-15,1.));
#11233=DIRECTION('ref_axis',(-1.,0.,0.));
#11234=DIRECTION('center_axis',(0.,1.,0.));
#11235=DIRECTION('ref_axis',(0.,0.,1.));
#11236=DIRECTION('center_axis',(0.,0.,1.));
#11237=DIRECTION('ref_axis',(-0.707106781186535,0.70710678118656,0.));
#11238=DIRECTION('',(0.,0.,1.));
#11239=DIRECTION('center_axis',(-0.816496580927727,0.40824829046386,-0.408248290463864));
#11240=DIRECTION('ref_axis',(-0.577350269189631,-0.577350269189623,0.577350269189623));
#11241=DIRECTION('center_axis',(0.,0.,1.));
#11242=DIRECTION('ref_axis',(0.,-1.,0.));
#11243=DIRECTION('center_axis',(-1.,0.,0.));
#11244=DIRECTION('ref_axis',(0.,0.,1.));
#11245=DIRECTION('center_axis',(0.,-1.,0.));
#11246=DIRECTION('ref_axis',(-1.,0.,0.));
#11247=DIRECTION('center_axis',(-1.,0.,0.));
#11248=DIRECTION('ref_axis',(0.,-0.707106781186551,0.707106781186544));
#11249=DIRECTION('',(-1.,0.,0.));
#11250=DIRECTION('center_axis',(0.,-1.,0.));
#11251=DIRECTION('ref_axis',(-0.707106781186544,0.,0.707106781186551));
#11252=DIRECTION('',(0.,1.,0.));
#11253=DIRECTION('',(0.,-1.,0.));
#11254=DIRECTION('center_axis',(-0.816496580927733,0.408248290463859,-0.408248290463852));
#11255=DIRECTION('ref_axis',(-0.577350269189616,-0.577350269189631,0.577350269189631));
#11256=DIRECTION('center_axis',(-1.,-1.77635683940023E-14,0.));
#11257=DIRECTION('ref_axis',(0.,0.,1.));
#11258=DIRECTION('center_axis',(0.,-1.,0.));
#11259=DIRECTION('ref_axis',(-1.,0.,0.));
#11260=DIRECTION('center_axis',(4.44089209850056E-15,0.,1.));
#11261=DIRECTION('ref_axis',(0.,-1.,0.));
#11262=DIRECTION('center_axis',(0.,-1.,0.));
#11263=DIRECTION('ref_axis',(-0.707106781186541,0.,0.707106781186554));
#11264=DIRECTION('',(0.,1.,0.));
#11265=DIRECTION('',(0.,-1.,0.));
#11266=DIRECTION('center_axis',(0.,0.,-1.));
#11267=DIRECTION('ref_axis',(-0.707106781186548,-0.707106781186548,0.));
#11268=DIRECTION('',(0.,0.,-1.));
#11269=DIRECTION('center_axis',(0.,1.,0.));
#11270=DIRECTION('ref_axis',(0.,0.,1.));
#11271=DIRECTION('center_axis',(-1.,0.,0.));
#11272=DIRECTION('ref_axis',(0.,0.,1.));
#11273=DIRECTION('center_axis',(0.,-1.,0.));
#11274=DIRECTION('ref_axis',(1.,0.,0.));
#11275=DIRECTION('center_axis',(0.,0.,1.));
#11276=DIRECTION('ref_axis',(0.,1.,0.));
#11277=DIRECTION('center_axis',(0.408248290463856,0.408248290463856,-0.816496580927733));
#11278=DIRECTION('ref_axis',(0.577350269189645,0.577350269189616,0.577350269189616));
#11279=DIRECTION('center_axis',(0.,1.,0.));
#11280=DIRECTION('ref_axis',(1.,0.,0.));
#11281=DIRECTION('center_axis',(1.,1.77635683940023E-14,0.));
#11282=DIRECTION('ref_axis',(0.,0.,1.));
#11283=DIRECTION('center_axis',(0.,-1.,0.));
#11284=DIRECTION('ref_axis',(0.,0.,-1.));
#11285=DIRECTION('center_axis',(0.,0.,1.));
#11286=DIRECTION('ref_axis',(-1.,0.,0.));
#11287=DIRECTION('center_axis',(0.,1.,0.));
#11288=DIRECTION('ref_axis',(0.,0.,-1.));
#11289=DIRECTION('center_axis',(-1.,0.,0.));
#11290=DIRECTION('ref_axis',(0.,-1.,0.));
#11291=DIRECTION('center_axis',(0.,0.,-1.));
#11292=DIRECTION('ref_axis',(-0.707106781186541,-0.707106781186554,0.));
#11293=DIRECTION('',(0.,0.,-1.));
#11294=DIRECTION('center_axis',(0.,-1.,0.));
#11295=DIRECTION('ref_axis',(0.707106781186547,0.,-0.707106781186548));
#11296=DIRECTION('',(0.,1.,0.));
#11297=DIRECTION('',(0.,-1.,0.));
#11298=DIRECTION('center_axis',(-0.816496580927733,-0.408248290463852,0.40824829046386));
#11299=DIRECTION('ref_axis',(0.577350269189623,-0.577350269189623,0.577350269189631));
#11300=DIRECTION('center_axis',(1.,0.,0.));
#11301=DIRECTION('ref_axis',(0.,-1.,0.));
#11302=DIRECTION('center_axis',(0.,-1.,0.));
#11303=DIRECTION('ref_axis',(0.,0.,1.));
#11304=DIRECTION('center_axis',(0.,1.,0.));
#11305=DIRECTION('ref_axis',(0.,0.,1.));
#11306=DIRECTION('center_axis',(0.,0.,1.));
#11307=DIRECTION('ref_axis',(1.,0.,0.));
#11308=DIRECTION('center_axis',(0.,-1.,0.));
#11309=DIRECTION('ref_axis',(0.,0.,-1.));
#11310=DIRECTION('center_axis',(1.,0.,0.));
#11311=DIRECTION('ref_axis',(0.,1.,0.));
#11312=DIRECTION('center_axis',(0.,-1.,0.));
#11313=DIRECTION('ref_axis',(0.,0.,-1.));
#11314=DIRECTION('center_axis',(1.,0.,0.));
#11315=DIRECTION('ref_axis',(0.,0.,1.));
#11316=DIRECTION('center_axis',(0.,1.,0.));
#11317=DIRECTION('ref_axis',(-1.,0.,0.));
#11318=DIRECTION('center_axis',(0.,0.,1.));
#11319=DIRECTION('ref_axis',(0.,-1.,0.));
#11320=DIRECTION('center_axis',(-1.,0.,0.));
#11321=DIRECTION('ref_axis',(0.,-0.707106781186553,0.707106781186542));
#11322=DIRECTION('',(-1.,0.,0.));
#11323=DIRECTION('center_axis',(0.,-1.,0.));
#11324=DIRECTION('ref_axis',(-0.707106781186546,0.,-0.707106781186549));
#11325=DIRECTION('',(0.,1.,0.));
#11326=DIRECTION('',(0.,-1.,0.));
#11327=DIRECTION('center_axis',(-0.816496580927737,0.408248290463858,0.408248290463847));
#11328=DIRECTION('ref_axis',(0.577350269189605,0.577350269189647,0.577350269189626));
#11329=DIRECTION('center_axis',(0.,0.,1.));
#11330=DIRECTION('ref_axis',(0.,1.,0.));
#11331=DIRECTION('center_axis',(1.,1.77635683940023E-14,0.));
#11332=DIRECTION('ref_axis',(0.,0.,1.));
#11333=DIRECTION('center_axis',(0.,1.,0.));
#11334=DIRECTION('ref_axis',(1.,0.,0.));
#11335=DIRECTION('center_axis',(0.408248290463859,-0.408248290463859,-0.81649658092773));
#11336=DIRECTION('ref_axis',(-0.577350269189628,0.577350269189628,-0.577350269189622));
#11337=DIRECTION('center_axis',(0.,0.,-1.));
#11338=DIRECTION('ref_axis',(0.,1.,0.));
#11339=DIRECTION('center_axis',(-1.,0.,0.));
#11340=DIRECTION('ref_axis',(0.,0.,-1.));
#11341=DIRECTION('center_axis',(0.,1.,0.));
#11342=DIRECTION('ref_axis',(-1.,0.,0.));
#11343=DIRECTION('center_axis',(-1.,0.,0.));
#11344=DIRECTION('ref_axis',(0.,0.707106781186553,-0.707106781186543));
#11345=DIRECTION('',(-1.,0.,0.));
#11346=DIRECTION('center_axis',(-0.816496580927728,-0.408248290463861,0.408248290463861));
#11347=DIRECTION('ref_axis',(0.577350269189631,-0.577350269189623,0.577350269189623));
#11348=DIRECTION('center_axis',(1.,0.,-8.88178419700124E-15));
#11349=DIRECTION('ref_axis',(0.,-1.,0.));
#11350=DIRECTION('center_axis',(0.,0.,1.));
#11351=DIRECTION('ref_axis',(1.,0.,0.));
#11352=DIRECTION('center_axis',(0.,-1.,0.));
#11353=DIRECTION('ref_axis',(0.,0.,1.));
#11354=DIRECTION('center_axis',(0.,0.,1.));
#11355=DIRECTION('ref_axis',(0.707106781186541,-0.707106781186554,0.));
#11356=DIRECTION('',(0.,0.,1.));
#11357=DIRECTION('center_axis',(0.,-1.,0.));
#11358=DIRECTION('ref_axis',(0.707106781186544,0.,0.707106781186551));
#11359=DIRECTION('',(0.,1.,0.));
#11360=DIRECTION('',(0.,-1.,0.));
#11361=DIRECTION('center_axis',(-0.816496580927738,0.408248290463855,0.408248290463848));
#11362=DIRECTION('ref_axis',(-0.577350269189624,-0.577350269189624,-0.577350269189629));
#11363=DIRECTION('center_axis',(0.,-1.,0.));
#11364=DIRECTION('ref_axis',(0.,0.,-1.));
#11365=DIRECTION('center_axis',(-1.,0.,1.77635683940025E-14));
#11366=DIRECTION('ref_axis',(0.,-1.,0.));
#11367=DIRECTION('center_axis',(0.,-1.,0.));
#11368=DIRECTION('ref_axis',(-0.70710678118654,0.,-0.707106781186555));
#11369=DIRECTION('',(0.,1.,0.));
#11370=DIRECTION('',(0.,-1.,0.));
#11371=DIRECTION('center_axis',(1.,0.,0.));
#11372=DIRECTION('ref_axis',(0.,-0.707106781186553,-0.707106781186543));
#11373=DIRECTION('',(1.,0.,0.));
#11374=DIRECTION('center_axis',(0.,1.,-3.55271367880045E-14));
#11375=DIRECTION('ref_axis',(0.,2.84217094304041E-14,1.));
#11376=DIRECTION('center_axis',(0.707106781186548,2.512147933894E-14,0.707106781186548));
#11377=DIRECTION('ref_axis',(0.707106781186548,0.,-0.707106781186548));
#11378=DIRECTION('center_axis',(0.,-1.,0.));
#11379=DIRECTION('ref_axis',(0.,0.,-1.));
#11380=DIRECTION('center_axis',(1.,0.,0.));
#11381=DIRECTION('ref_axis',(0.,1.,0.));
#11382=DIRECTION('center_axis',(-0.816496580927733,-0.408248290463852,-0.40824829046386));
#11383=DIRECTION('ref_axis',(-0.577350269189623,0.577350269189623,0.577350269189631));
#11384=DIRECTION('center_axis',(-1.,0.,0.));
#11385=DIRECTION('ref_axis',(0.,1.,0.));
#11386=DIRECTION('center_axis',(0.,1.,0.));
#11387=DIRECTION('ref_axis',(0.,0.,1.));
#11388=DIRECTION('center_axis',(0.,0.,1.));
#11389=DIRECTION('ref_axis',(-0.707106781186548,0.707106781186548,0.));
#11390=DIRECTION('',(0.,0.,1.));
#11391=DIRECTION('center_axis',(0.,1.,0.));
#11392=DIRECTION('ref_axis',(0.,0.,1.));
#11393=DIRECTION('center_axis',(1.,0.,0.));
#11394=DIRECTION('ref_axis',(0.,0.,1.));
#11395=DIRECTION('center_axis',(0.,1.,0.));
#11396=DIRECTION('ref_axis',(-0.707106781186548,0.,0.707106781186548));
#11397=DIRECTION('center_axis',(0.707106781186554,0.,0.707106781186541));
#11398=DIRECTION('ref_axis',(0.,-1.,0.));
#11399=DIRECTION('center_axis',(-0.408248290463856,-0.408248290463856,-0.816496580927733));
#11400=DIRECTION('ref_axis',(-0.577350269189645,-0.577350269189616,0.577350269189616));
#11401=DIRECTION('center_axis',(0.,-1.,0.));
#11402=DIRECTION('ref_axis',(-1.,0.,0.));
#11403=DIRECTION('center_axis',(0.,0.,1.));
#11404=DIRECTION('ref_axis',(0.,-1.,0.));
#11405=DIRECTION('center_axis',(-1.,-1.77635683940023E-14,0.));
#11406=DIRECTION('ref_axis',(0.,0.,1.));
#11407=DIRECTION('center_axis',(0.,0.,1.));
#11408=DIRECTION('ref_axis',(-0.707106781186548,-0.707106781186548,0.));
#11409=DIRECTION('center_axis',(-0.827465426020369,0.538877990790914,0.157833709270475));
#11410=DIRECTION('ref_axis',(0.561516668266342,0.794104487760818,0.232587819494476));
#11411=DIRECTION('center_axis',(0.,1.,0.));
#11412=DIRECTION('ref_axis',(0.707106781186548,0.,-0.707106781186548));
#11413=DIRECTION('center_axis',(0.707106781186548,0.,0.707106781186548));
#11414=DIRECTION('ref_axis',(0.,1.,0.));
#11415=DIRECTION('center_axis',(1.,0.,0.));
#11416=DIRECTION('ref_axis',(0.,0.,1.));
#11417=DIRECTION('center_axis',(-0.707106781186548,0.,-0.707106781186548));
#11418=DIRECTION('ref_axis',(0.499999999999996,0.707106781186553,-0.499999999999996));
#11419=DIRECTION('',(-0.707106781186548,0.,-0.707106781186548));
#11420=DIRECTION('center_axis',(-1.,0.,0.));
#11421=DIRECTION('ref_axis',(0.,0.707106781186551,0.707106781186544));
#11422=DIRECTION('',(1.,0.,0.));
#11423=DIRECTION('center_axis',(-0.827465426020366,-0.538877990790921,0.15783370927047));
#11424=DIRECTION('ref_axis',(0.561516668266338,-0.794104487760823,0.23258781949447));
#11425=DIRECTION('center_axis',(0.707106781186548,0.,0.707106781186548));
#11426=DIRECTION('ref_axis',(0.707106781186548,0.,-0.707106781186548));
#11427=DIRECTION('center_axis',(0.,-1.,0.));
#11428=DIRECTION('ref_axis',(0.,0.,1.));
#11429=DIRECTION('center_axis',(1.,0.,0.));
#11430=DIRECTION('ref_axis',(0.,-1.,0.));
#11431=DIRECTION('center_axis',(0.,1.,0.));
#11432=DIRECTION('ref_axis',(0.923879532511288,0.,0.382683432365088));
#11433=DIRECTION('',(0.,-1.,0.));
#11434=DIRECTION('',(0.,1.,0.));
#11435=DIRECTION('center_axis',(1.,0.,0.));
#11436=DIRECTION('ref_axis',(0.,-0.707106781186551,0.707106781186544));
#11437=DIRECTION('',(-1.,0.,0.));
#11438=DIRECTION('center_axis',(0.707106781186548,0.,0.707106781186548));
#11439=DIRECTION('ref_axis',(0.499999999999996,-0.707106781186553,-0.499999999999996));
#11440=DIRECTION('',(0.707106781186548,0.,0.707106781186548));
#11441=DIRECTION('center_axis',(0.,-1.,0.));
#11442=DIRECTION('ref_axis',(-0.707106781186538,0.,0.707106781186557));
#11443=DIRECTION('',(0.,1.,0.));
#11444=DIRECTION('center_axis',(-1.,0.,0.));
#11445=DIRECTION('ref_axis',(0.,-0.707106781186551,0.707106781186544));
#11446=DIRECTION('',(-1.,0.,0.));
#11447=DIRECTION('center_axis',(0.,-1.,0.));
#11448=DIRECTION('ref_axis',(-0.923879532511288,0.,-0.382683432365088));
#11449=DIRECTION('',(0.,1.,0.));
#11450=DIRECTION('',(0.,-1.,0.));
#11451=DIRECTION('center_axis',(1.,0.,0.));
#11452=DIRECTION('ref_axis',(0.,0.707106781186551,0.707106781186544));
#11453=DIRECTION('',(1.,0.,0.));
#11454=DIRECTION('center_axis',(0.,0.,-1.));
#11455=DIRECTION('ref_axis',(0.707106781186548,0.707106781186548,0.));
#11456=DIRECTION('',(0.,0.,-1.));
#11457=DIRECTION('center_axis',(1.,0.,0.));
#11458=DIRECTION('ref_axis',(0.,0.707106781186553,0.707106781186542));
#11459=DIRECTION('',(1.,0.,0.));
#11460=DIRECTION('center_axis',(0.,1.,0.));
#11461=DIRECTION('ref_axis',(0.707106781186538,0.,0.707106781186557));
#11462=DIRECTION('',(0.,-1.,0.));
#11463=DIRECTION('center_axis',(1.,0.,0.));
#11464=DIRECTION('ref_axis',(0.,-0.707106781186551,0.707106781186544));
#11465=DIRECTION('',(-1.,0.,0.));
#11466=DIRECTION('center_axis',(-1.,0.,0.));
#11467=DIRECTION('ref_axis',(0.,0.707106781186551,0.707106781186544));
#11468=DIRECTION('',(1.,0.,0.));
#11469=DIRECTION('center_axis',(0.,0.,1.));
#11470=DIRECTION('ref_axis',(-0.707106781186541,0.707106781186554,0.));
#11471=DIRECTION('',(0.,0.,1.));
#11472=DIRECTION('center_axis',(1.,0.,0.));
#11473=DIRECTION('ref_axis',(0.,0.707106781186551,0.707106781186544));
#11474=DIRECTION('',(1.,0.,0.));
#11475=DIRECTION('center_axis',(0.,-1.,0.));
#11476=DIRECTION('ref_axis',(0.707106781186538,0.,-0.707106781186557));
#11477=DIRECTION('',(0.,1.,0.));
#11478=DIRECTION('',(0.,-1.,0.));
#11479=DIRECTION('center_axis',(0.,0.,1.));
#11480=DIRECTION('ref_axis',(1.,0.,0.));
#11481=DIRECTION('center_axis',(1.,0.,0.));
#11482=DIRECTION('ref_axis',(0.,0.,1.));
#11483=DIRECTION('center_axis',(0.,0.,-1.));
#11484=DIRECTION('ref_axis',(1.,0.,0.));
#11485=DIRECTION('center_axis',(1.,0.,0.));
#11486=DIRECTION('ref_axis',(0.,0.,1.));
#11487=DIRECTION('center_axis',(0.,0.,-1.));
#11488=DIRECTION('ref_axis',(1.,0.,0.));
#11489=DIRECTION('center_axis',(-1.,0.,0.));
#11490=DIRECTION('ref_axis',(0.,0.,-1.));
#11491=DIRECTION('center_axis',(0.,0.,-1.));
#11492=DIRECTION('ref_axis',(1.,0.,0.));
#11493=DIRECTION('center_axis',(-1.,0.,0.));
#11494=DIRECTION('ref_axis',(0.,-1.,0.));
#11495=DIRECTION('center_axis',(-0.707106781186548,0.,0.707106781186548));
#11496=DIRECTION('ref_axis',(-0.707106781186548,0.,-0.707106781186548));
#11497=DIRECTION('center_axis',(0.,0.,1.));
#11498=DIRECTION('ref_axis',(1.,0.,0.));
#11499=DIRECTION('center_axis',(0.,0.,1.));
#11500=DIRECTION('ref_axis',(1.,0.,0.));
#11501=DIRECTION('axis',(0.,0.,1.));
#11502=DIRECTION('refdir',(1.,0.,0.));
#11503=DIRECTION('center_axis',(0.,0.,-1.));
#11504=DIRECTION('ref_axis',(-1.,0.,0.));
#11505=DIRECTION('center_axis',(0.,0.,-1.));
#11506=DIRECTION('ref_axis',(-1.,0.,0.));
#11507=DIRECTION('',(0.,0.,-1.));
#11508=DIRECTION('center_axis',(0.,0.,1.));
#11509=DIRECTION('ref_axis',(-1.,0.,0.));
#11510=DIRECTION('center_axis',(0.,0.,-1.));
#11511=DIRECTION('ref_axis',(-1.,0.,0.));
#11512=DIRECTION('center_axis',(0.,0.,-1.));
#11513=DIRECTION('ref_axis',(-1.,0.,0.));
#11514=DIRECTION('',(0.,0.,-1.));
#11515=DIRECTION('center_axis',(0.,0.,-1.));
#11516=DIRECTION('ref_axis',(-1.,0.,0.));
#11517=DIRECTION('center_axis',(0.,0.,1.));
#11518=DIRECTION('ref_axis',(-1.,0.,0.));
#11519=DIRECTION('center_axis',(0.,0.,-1.));
#11520=DIRECTION('ref_axis',(-1.,0.,0.));
#11521=DIRECTION('center_axis',(0.,0.,-1.));
#11522=DIRECTION('ref_axis',(-1.,0.,0.));
#11523=DIRECTION('',(0.,0.,-1.));
#11524=DIRECTION('center_axis',(0.,0.,-1.));
#11525=DIRECTION('ref_axis',(-1.,0.,0.));
#11526=DIRECTION('center_axis',(0.,0.,1.));
#11527=DIRECTION('ref_axis',(-1.,0.,0.));
#11528=DIRECTION('center_axis',(0.,0.,-1.));
#11529=DIRECTION('ref_axis',(-1.,0.,0.));
#11530=DIRECTION('center_axis',(0.,0.,-1.));
#11531=DIRECTION('ref_axis',(-1.,0.,0.));
#11532=DIRECTION('',(0.,0.,-1.));
#11533=DIRECTION('center_axis',(0.,0.,1.));
#11534=DIRECTION('ref_axis',(-1.,0.,0.));
#11535=DIRECTION('center_axis',(-0.827465426020391,-0.538877990790891,0.15783370927044));
#11536=DIRECTION('ref_axis',(-0.561516668266297,0.79410448776086,-0.232587819494442));
#11537=DIRECTION('center_axis',(7.105427357601E-14,1.,7.105427357601E-14));
#11538=DIRECTION('ref_axis',(-0.707106781186548,0.,0.707106781186548));
#11539=DIRECTION('center_axis',(-0.707106781186552,0.,-0.707106781186543));
#11540=DIRECTION('ref_axis',(0.,1.,0.));
#11541=DIRECTION('center_axis',(-1.,0.,0.));
#11542=DIRECTION('ref_axis',(0.,0.,-1.));
#11543=DIRECTION('center_axis',(-0.827465426020364,0.53887799079092,0.157833709270477));
#11544=DIRECTION('ref_axis',(-0.561516668266353,-0.794104487760813,-0.232587819494468));
#11545=DIRECTION('center_axis',(-1.,0.,0.));
#11546=DIRECTION('ref_axis',(0.,-1.,0.));
#11547=DIRECTION('center_axis',(-0.707106781186548,0.,-0.707106781186548));
#11548=DIRECTION('ref_axis',(-0.707106781186548,0.,0.707106781186548));
#11549=DIRECTION('center_axis',(0.,-1.,0.));
#11550=DIRECTION('ref_axis',(0.,0.,-1.));
#11551=DIRECTION('center_axis',(0.,-1.,0.));
#11552=DIRECTION('ref_axis',(0.,0.,-1.));
#11553=DIRECTION('center_axis',(0.,-1.,0.));
#11554=DIRECTION('ref_axis',(0.,0.,1.));
#11555=DIRECTION('center_axis',(-1.,0.,0.));
#11556=DIRECTION('ref_axis',(0.,1.,0.));
#11557=DIRECTION('center_axis',(0.,1.,0.));
#11558=DIRECTION('ref_axis',(0.707106781186549,0.,0.707106781186546));
#11559=DIRECTION('center_axis',(0.,0.,-1.));
#11560=DIRECTION('ref_axis',(-1.,0.,0.));
#11561=DIRECTION('center_axis',(1.,0.,0.));
#11562=DIRECTION('ref_axis',(0.,0.707106781186554,-0.707106781186541));
#11563=DIRECTION('',(-1.,0.,0.));
#11564=DIRECTION('',(1.,0.,0.));
#11565=DIRECTION('center_axis',(0.,-1.,3.5527136788003E-14));
#11566=DIRECTION('ref_axis',(0.,-2.84217094304039E-14,-1.));
#11567=DIRECTION('center_axis',(0.,1.,0.));
#11568=DIRECTION('ref_axis',(0.923879532511286,0.,0.382683432365093));
#11569=DIRECTION('center_axis',(-0.707106781186543,-2.51214793389392E-14,
-0.707106781186552));
#11570=DIRECTION('ref_axis',(-0.707106781186552,0.,0.707106781186543));
#11571=DIRECTION('center_axis',(-5.02429586778809E-14,-1.,0.));
#11572=DIRECTION('ref_axis',(0.,0.,1.));
#11573=DIRECTION('center_axis',(-1.,0.,0.));
#11574=DIRECTION('ref_axis',(0.,1.,0.));
#11575=DIRECTION('center_axis',(0.,1.,0.));
#11576=DIRECTION('ref_axis',(0.,0.,1.));
#11577=DIRECTION('center_axis',(0.,1.,0.));
#11578=DIRECTION('ref_axis',(1.,0.,0.));
#11579=DIRECTION('center_axis',(0.,0.,-1.));
#11580=DIRECTION('ref_axis',(0.,-1.,0.));
#11581=DIRECTION('center_axis',(0.,-1.,0.));
#11582=DIRECTION('ref_axis',(0.707106781186549,0.,0.707106781186546));
#11583=DIRECTION('center_axis',(-1.,0.,0.));
#11584=DIRECTION('ref_axis',(0.,0.,-1.));
#11585=DIRECTION('center_axis',(0.,1.,0.));
#11586=DIRECTION('ref_axis',(0.,0.,1.));
#11587=DIRECTION('center_axis',(0.,-1.,0.));
#11588=DIRECTION('ref_axis',(0.9238795325113,0.,0.382683432365059));
#11589=DIRECTION('center_axis',(-1.,0.,0.));
#11590=DIRECTION('ref_axis',(0.,0.,-1.));
#11591=DIRECTION('center_axis',(0.,1.,0.));
#11592=DIRECTION('ref_axis',(0.707106781186548,0.,-0.707106781186548));
#11593=DIRECTION('center_axis',(-0.707106781186539,0.,-0.707106781186556));
#11594=DIRECTION('ref_axis',(0.,-1.,0.));
#11595=DIRECTION('center_axis',(0.707106781186548,0.,0.707106781186548));
#11596=DIRECTION('ref_axis',(-0.499999999999994,-0.707106781186551,0.500000000000001));
#11597=DIRECTION('',(-0.707106781186548,0.,-0.707106781186548));
#11598=DIRECTION('',(0.707106781186548,0.,0.707106781186548));
#11599=DIRECTION('center_axis',(-0.816496580927733,-0.408248290463856,0.408248290463857));
#11600=DIRECTION('ref_axis',(-0.577350269189618,0.57735026918964,-0.577350269189619));
#11601=DIRECTION('center_axis',(0.,1.,0.));
#11602=DIRECTION('ref_axis',(-1.,0.,0.));
#11603=DIRECTION('center_axis',(0.,0.,-1.));
#11604=DIRECTION('ref_axis',(0.,1.,0.));
#11605=DIRECTION('center_axis',(-1.,0.,0.));
#11606=DIRECTION('ref_axis',(0.,0.,-1.));
#11607=DIRECTION('center_axis',(0.,0.,-1.));
#11608=DIRECTION('ref_axis',(-0.707106781186541,0.707106781186554,0.));
#11609=DIRECTION('',(0.,0.,1.));
#11610=DIRECTION('',(0.,0.,-1.));
#11611=DIRECTION('center_axis',(0.408248290463858,-0.408248290463858,-0.816496580927731));
#11612=DIRECTION('ref_axis',(-0.577350269189628,0.577350269189628,-0.577350269189621));
#11613=DIRECTION('center_axis',(0.,0.,-1.));
#11614=DIRECTION('ref_axis',(0.,1.,0.));
#11615=DIRECTION('center_axis',(-1.,0.,0.));
#11616=DIRECTION('ref_axis',(0.,0.,-1.));
#11617=DIRECTION('center_axis',(0.,1.,0.));
#11618=DIRECTION('ref_axis',(-1.,0.,0.));
#11619=DIRECTION('center_axis',(-1.,0.,0.));
#11620=DIRECTION('ref_axis',(0.,0.707106781186554,-0.707106781186541));
#11621=DIRECTION('',(1.,0.,0.));
#11622=DIRECTION('',(-1.,0.,0.));
#11623=DIRECTION('center_axis',(-0.816496580927731,0.408248290463855,0.40824829046386));
#11624=DIRECTION('ref_axis',(-0.577350269189618,-0.577350269189639,-0.57735026918962));
#11625=DIRECTION('center_axis',(0.,-1.,0.));
#11626=DIRECTION('ref_axis',(0.,0.,-1.));
#11627=DIRECTION('center_axis',(-1.,0.,0.));
#11628=DIRECTION('ref_axis',(0.,-1.,0.));
#11629=DIRECTION('center_axis',(0.,0.,-1.));
#11630=DIRECTION('ref_axis',(-1.,0.,0.));
#11631=DIRECTION('center_axis',(0.408248290463854,0.408248290463854,-0.816496580927736));
#11632=DIRECTION('ref_axis',(-0.577350269189645,-0.577350269189616,-0.577350269189616));
#11633=DIRECTION('center_axis',(0.,-1.,0.));
#11634=DIRECTION('ref_axis',(0.,0.,-1.));
#11635=DIRECTION('center_axis',(-1.,0.,1.77635683940026E-14));
#11636=DIRECTION('ref_axis',(0.,-1.,0.));
#11637=DIRECTION('center_axis',(0.,0.,-1.));
#11638=DIRECTION('ref_axis',(-1.,0.,0.));
#11639=DIRECTION('center_axis',(1.,0.,0.));
#11640=DIRECTION('ref_axis',(0.,-0.707106781186554,-0.707106781186541));
#11641=DIRECTION('',(-1.,0.,0.));
#11642=DIRECTION('',(1.,0.,0.));
#11643=DIRECTION('center_axis',(-0.816496580927732,0.408248290463855,-0.408248290463859));
#11644=DIRECTION('ref_axis',(0.577350269189618,0.57735026918964,-0.577350269189619));
#11645=DIRECTION('center_axis',(0.,1.,0.));
#11646=DIRECTION('ref_axis',(0.,0.,-1.));
#11647=DIRECTION('center_axis',(1.,0.,0.));
#11648=DIRECTION('ref_axis',(0.,1.,0.));
#11649=DIRECTION('center_axis',(0.,-2.22044604925028E-15,-1.));
#11650=DIRECTION('ref_axis',(1.,0.,0.));
#11651=DIRECTION('center_axis',(1.,0.,0.));
#11652=DIRECTION('ref_axis',(0.,0.707106781186553,-0.707106781186542));
#11653=DIRECTION('',(-1.,0.,0.));
#11654=DIRECTION('',(1.,0.,0.));
#11655=DIRECTION('center_axis',(-0.816496580927724,-0.408248290463876,-0.408248290463855));
#11656=DIRECTION('ref_axis',(-0.577350269189633,0.577350269189633,0.577350269189612));
#11657=DIRECTION('center_axis',(-1.,0.,0.));
#11658=DIRECTION('ref_axis',(0.,1.,0.));
#11659=DIRECTION('center_axis',(0.,0.,1.));
#11660=DIRECTION('ref_axis',(-1.,0.,0.));
#11661=DIRECTION('center_axis',(0.,1.,0.));
#11662=DIRECTION('ref_axis',(0.,0.,1.));
#11663=DIRECTION('center_axis',(0.,0.,1.));
#11664=DIRECTION('ref_axis',(-0.707106781186548,0.707106781186548,0.));
#11665=DIRECTION('',(0.,0.,-1.));
#11666=DIRECTION('',(0.,0.,1.));
#11667=DIRECTION('center_axis',(-0.816496580927732,-0.408248290463855,-0.408248290463859));
#11668=DIRECTION('ref_axis',(0.577350269189618,-0.57735026918964,-0.577350269189619));
#11669=DIRECTION('center_axis',(0.,-1.,0.));
#11670=DIRECTION('ref_axis',(1.,0.,0.));
#11671=DIRECTION('center_axis',(2.22044604925032E-15,0.,-1.));
#11672=DIRECTION('ref_axis',(0.,-1.,0.));
#11673=DIRECTION('center_axis',(1.,0.,0.));
#11674=DIRECTION('ref_axis',(0.,0.,-1.));
#11675=DIRECTION('center_axis',(-0.408248290463854,-0.408248290463854,-0.816496580927736));
#11676=DIRECTION('ref_axis',(-0.577350269189645,-0.577350269189616,0.577350269189616));
#11677=DIRECTION('center_axis',(0.,-1.,0.));
#11678=DIRECTION('ref_axis',(-1.,0.,0.));
#11679=DIRECTION('center_axis',(0.,0.,1.));
#11680=DIRECTION('ref_axis',(0.,-1.,0.));
#11681=DIRECTION('center_axis',(-1.,-1.77635683940023E-14,0.));
#11682=DIRECTION('ref_axis',(0.,0.,1.));
#11683=DIRECTION('center_axis',(0.,0.,1.));
#11684=DIRECTION('ref_axis',(-0.707106781186548,-0.707106781186548,0.));
#11685=DIRECTION('',(0.,0.,-1.));
#11686=DIRECTION('',(0.,0.,1.));
#11687=DIRECTION('center_axis',(0.,-1.,0.));
#11688=DIRECTION('ref_axis',(0.,0.,-1.));
#11689=DIRECTION('center_axis',(0.,-1.,0.));
#11690=DIRECTION('ref_axis',(-1.,0.,0.));
#11691=DIRECTION('center_axis',(0.,0.,-1.));
#11692=DIRECTION('ref_axis',(0.,1.,0.));
#11693=DIRECTION('center_axis',(0.,1.,0.));
#11694=DIRECTION('ref_axis',(-0.707106781186546,0.,0.707106781186549));
#11695=DIRECTION('center_axis',(1.,0.,0.));
#11696=DIRECTION('ref_axis',(0.,0.,-1.));
#11697=DIRECTION('center_axis',(0.,0.,1.));
#11698=DIRECTION('ref_axis',(0.707106781186541,0.707106781186554,0.));
#11699=DIRECTION('',(0.,0.,-1.));
#11700=DIRECTION('',(0.,0.,1.));
#11701=DIRECTION('center_axis',(0.408248290463854,0.408248290463854,-0.816496580927736));
#11702=DIRECTION('ref_axis',(0.577350269189645,0.577350269189616,0.577350269189616));
#11703=DIRECTION('center_axis',(0.,1.,0.));
#11704=DIRECTION('ref_axis',(1.,0.,0.));
#11705=DIRECTION('center_axis',(0.,0.,1.));
#11706=DIRECTION('ref_axis',(0.,1.,0.));
#11707=DIRECTION('center_axis',(1.,1.77635683940023E-14,0.));
#11708=DIRECTION('ref_axis',(0.,0.,1.));
#11709=DIRECTION('center_axis',(0.,1.,0.));
#11710=DIRECTION('ref_axis',(0.,0.,1.));
#11711=DIRECTION('center_axis',(0.,1.,0.));
#11712=DIRECTION('ref_axis',(0.,0.,1.));
#11713=DIRECTION('center_axis',(1.,0.,0.));
#11714=DIRECTION('ref_axis',(0.,-1.,0.));
#11715=DIRECTION('center_axis',(0.,-1.,0.));
#11716=DIRECTION('ref_axis',(-0.707106781186549,0.,0.707106781186546));
#11717=DIRECTION('center_axis',(0.,0.,-1.));
#11718=DIRECTION('ref_axis',(1.,0.,0.));
#11719=DIRECTION('center_axis',(-0.816496580927724,-0.408248290463876,0.408248290463855));
#11720=DIRECTION('ref_axis',(0.577350269189633,-0.577350269189633,0.577350269189612));
#11721=DIRECTION('center_axis',(1.,0.,0.));
#11722=DIRECTION('ref_axis',(0.,-1.,0.));
#11723=DIRECTION('center_axis',(0.,0.,1.));
#11724=DIRECTION('ref_axis',(1.,0.,0.));
#11725=DIRECTION('center_axis',(0.,-1.,0.));
#11726=DIRECTION('ref_axis',(0.,0.,1.));
#11727=DIRECTION('center_axis',(-0.408248290463855,-0.408248290463855,-0.816496580927734));
#11728=DIRECTION('ref_axis',(0.577350269189645,0.577350269189616,-0.577350269189616));
#11729=DIRECTION('center_axis',(0.,1.,0.));
#11730=DIRECTION('ref_axis',(0.,0.,-1.));
#11731=DIRECTION('center_axis',(1.,0.,1.77635683940026E-14));
#11732=DIRECTION('ref_axis',(0.,1.,0.));
#11733=DIRECTION('center_axis',(0.,0.,-1.));
#11734=DIRECTION('ref_axis',(1.,0.,0.));
#11735=DIRECTION('center_axis',(1.,0.,0.));
#11736=DIRECTION('ref_axis',(0.,0.707106781186554,-0.707106781186541));
#11737=DIRECTION('',(-1.,0.,0.));
#11738=DIRECTION('',(1.,0.,0.));
#11739=DIRECTION('center_axis',(-0.816496580927728,0.408248290463864,-0.408248290463857));
#11740=DIRECTION('ref_axis',(0.577350269189626,0.577350269189626,-0.577350269189626));
#11741=DIRECTION('center_axis',(0.,0.,-1.));
#11742=DIRECTION('ref_axis',(1.,0.,0.));
#11743=DIRECTION('center_axis',(0.,1.,0.));
#11744=DIRECTION('ref_axis',(0.,0.,-1.));
#11745=DIRECTION('center_axis',(1.,0.,1.77635683940026E-14));
#11746=DIRECTION('ref_axis',(0.,1.,0.));
#11747=DIRECTION('center_axis',(-0.408248290463855,0.408248290463855,-0.816496580927734));
#11748=DIRECTION('ref_axis',(0.577350269189645,-0.577350269189616,-0.577350269189616));
#11749=DIRECTION('center_axis',(0.,-1.,0.));
#11750=DIRECTION('ref_axis',(1.,0.,0.));
#11751=DIRECTION('center_axis',(0.,0.,-1.));
#11752=DIRECTION('ref_axis',(0.,-1.,0.));
#11753=DIRECTION('center_axis',(1.,0.,0.));
#11754=DIRECTION('ref_axis',(0.,0.,-1.));
#11755=DIRECTION('center_axis',(-0.408248290463858,0.408248290463858,-0.816496580927731));
#11756=DIRECTION('ref_axis',(0.577350269189628,-0.577350269189628,-0.577350269189621));
#11757=DIRECTION('center_axis',(0.,0.,-1.));
#11758=DIRECTION('ref_axis',(0.,-1.,0.));
#11759=DIRECTION('center_axis',(1.,0.,0.));
#11760=DIRECTION('ref_axis',(0.,0.,-1.));
#11761=DIRECTION('center_axis',(0.,-1.,0.));
#11762=DIRECTION('ref_axis',(1.,0.,0.));
#11763=DIRECTION('center_axis',(0.,-1.,0.));
#11764=DIRECTION('ref_axis',(0.,0.,-1.));
#11765=DIRECTION('center_axis',(0.,-1.,0.));
#11766=DIRECTION('ref_axis',(-1.,0.,0.));
#11767=DIRECTION('center_axis',(0.,0.,-1.));
#11768=DIRECTION('ref_axis',(0.,1.,0.));
#11769=DIRECTION('center_axis',(0.,1.,0.));
#11770=DIRECTION('ref_axis',(-0.707106781186548,0.,0.707106781186548));
#11771=DIRECTION('center_axis',(1.,0.,0.));
#11772=DIRECTION('ref_axis',(0.,0.,-1.));
#11773=DIRECTION('center_axis',(0.,0.,1.));
#11774=DIRECTION('ref_axis',(0.707106781186548,0.707106781186548,0.));
#11775=DIRECTION('',(0.,0.,-1.));
#11776=DIRECTION('',(0.,0.,1.));
#11777=DIRECTION('center_axis',(-1.,0.,0.));
#11778=DIRECTION('ref_axis',(0.,0.707106781186554,-0.707106781186541));
#11779=DIRECTION('',(1.,0.,0.));
#11780=DIRECTION('',(-1.,0.,0.));
#11781=DIRECTION('center_axis',(0.,1.,0.));
#11782=DIRECTION('ref_axis',(0.,0.,1.));
#11783=DIRECTION('center_axis',(0.,1.,0.));
#11784=DIRECTION('ref_axis',(0.,0.,1.));
#11785=DIRECTION('center_axis',(1.,0.,0.));
#11786=DIRECTION('ref_axis',(0.,-1.,0.));
#11787=DIRECTION('center_axis',(0.,-1.,0.));
#11788=DIRECTION('ref_axis',(-0.707106781186548,0.,0.707106781186548));
#11789=DIRECTION('center_axis',(0.,0.,-1.));
#11790=DIRECTION('ref_axis',(1.,0.,0.));
#11791=DIRECTION('center_axis',(1.,0.,0.));
#11792=DIRECTION('ref_axis',(0.,-0.707106781186554,-0.707106781186541));
#11793=DIRECTION('',(-1.,0.,0.));
#11794=DIRECTION('',(1.,0.,0.));
#11795=DIRECTION('center_axis',(0.,0.,-1.));
#11796=DIRECTION('ref_axis',(0.707106781186548,-0.707106781186548,0.));
#11797=DIRECTION('',(0.,0.,1.));
#11798=DIRECTION('',(0.,0.,-1.));
#11799=DIRECTION('center_axis',(0.,1.,0.));
#11800=DIRECTION('ref_axis',(-0.707106781186541,0.,0.707106781186554));
#11801=DIRECTION('',(0.,-1.,0.));
#11802=DIRECTION('',(0.,1.,0.));
#11803=DIRECTION('center_axis',(0.,1.,0.));
#11804=DIRECTION('ref_axis',(0.707106781186541,0.,-0.707106781186554));
#11805=DIRECTION('',(0.,-1.,0.));
#11806=DIRECTION('',(0.,1.,0.));
#11807=DIRECTION('center_axis',(0.,0.,1.));
#11808=DIRECTION('ref_axis',(0.707106781186548,-0.707106781186548,0.));
#11809=DIRECTION('',(0.,0.,-1.));
#11810=DIRECTION('',(0.,0.,1.));
#11811=DIRECTION('center_axis',(-1.,0.,0.));
#11812=DIRECTION('ref_axis',(0.,-0.707106781186554,-0.707106781186541));
#11813=DIRECTION('',(1.,0.,0.));
#11814=DIRECTION('',(-1.,0.,0.));
#11815=DIRECTION('center_axis',(0.,-1.,0.));
#11816=DIRECTION('ref_axis',(0.707106781186541,0.,-0.707106781186554));
#11817=DIRECTION('',(0.,1.,0.));
#11818=DIRECTION('',(0.,-1.,0.));
#11819=DIRECTION('center_axis',(0.,0.,1.));
#11820=DIRECTION('ref_axis',(0.707106781186548,0.707106781186548,0.));
#11821=DIRECTION('',(0.,0.,-1.));
#11822=DIRECTION('',(0.,0.,1.));
#11823=DIRECTION('center_axis',(0.,1.,0.));
#11824=DIRECTION('ref_axis',(0.707106781186541,0.,0.707106781186554));
#11825=DIRECTION('',(0.,-1.,0.));
#11826=DIRECTION('',(0.,1.,0.));
#11827=DIRECTION('center_axis',(1.,0.,0.));
#11828=DIRECTION('ref_axis',(0.,-0.707106781186554,0.707106781186541));
#11829=DIRECTION('',(-1.,0.,0.));
#11830=DIRECTION('',(1.,0.,0.));
#11831=DIRECTION('center_axis',(0.,0.,-1.));
#11832=DIRECTION('ref_axis',(0.707106781186541,-0.707106781186554,0.));
#11833=DIRECTION('',(0.,0.,1.));
#11834=DIRECTION('',(0.,0.,-1.));
#11835=DIRECTION('center_axis',(0.,-1.,0.));
#11836=DIRECTION('ref_axis',(-0.707106781186544,0.,0.707106781186551));
#11837=DIRECTION('',(0.,1.,0.));
#11838=DIRECTION('',(0.,-1.,0.));
#11839=DIRECTION('center_axis',(-1.,0.,0.));
#11840=DIRECTION('ref_axis',(0.,0.707106781186554,0.707106781186541));
#11841=DIRECTION('',(1.,0.,0.));
#11842=DIRECTION('',(-1.,0.,0.));
#11843=DIRECTION('center_axis',(0.,-1.,0.));
#11844=DIRECTION('ref_axis',(-0.707106781186541,0.,0.707106781186554));
#11845=DIRECTION('',(0.,1.,0.));
#11846=DIRECTION('',(0.,-1.,0.));
#11847=DIRECTION('center_axis',(-1.,0.,0.));
#11848=DIRECTION('ref_axis',(0.,-0.707106781186553,-0.707106781186542));
#11849=DIRECTION('',(1.,0.,0.));
#11850=DIRECTION('',(-1.,0.,0.));
#11851=DIRECTION('center_axis',(0.,-1.,0.));
#11852=DIRECTION('ref_axis',(0.707106781186546,0.,-0.707106781186549));
#11853=DIRECTION('',(0.,1.,0.));
#11854=DIRECTION('',(0.,-1.,0.));
#11855=DIRECTION('center_axis',(0.,-1.,0.));
#11856=DIRECTION('ref_axis',(-0.707106781186541,0.,-0.707106781186554));
#11857=DIRECTION('',(0.,1.,0.));
#11858=DIRECTION('',(0.,-1.,0.));
#11859=DIRECTION('center_axis',(0.,0.,1.));
#11860=DIRECTION('ref_axis',(-0.707106781186541,-0.707106781186554,0.));
#11861=DIRECTION('',(0.,0.,-1.));
#11862=DIRECTION('',(0.,0.,1.));
#11863=DIRECTION('center_axis',(0.,-1.,0.));
#11864=DIRECTION('ref_axis',(-0.707106781186547,0.,-0.707106781186548));
#11865=DIRECTION('',(0.,1.,0.));
#11866=DIRECTION('',(0.,-1.,0.));
#11867=DIRECTION('center_axis',(0.,-1.,0.));
#11868=DIRECTION('ref_axis',(0.923879532511288,0.,0.382683432365088));
#11869=DIRECTION('',(0.,1.,0.));
#11870=DIRECTION('',(0.,-1.,0.));
#11871=DIRECTION('center_axis',(-1.,0.,0.));
#11872=DIRECTION('ref_axis',(0.,-0.707106781186554,-0.707106781186541));
#11873=DIRECTION('',(1.,0.,0.));
#11874=DIRECTION('',(-1.,0.,0.));
#11875=DIRECTION('center_axis',(0.,-1.,0.));
#11876=DIRECTION('ref_axis',(0.707106781186548,0.,0.707106781186548));
#11877=DIRECTION('',(0.,1.,0.));
#11878=DIRECTION('',(0.,-1.,0.));
#11879=DIRECTION('center_axis',(-0.707106781186548,0.,-0.707106781186548));
#11880=DIRECTION('ref_axis',(-0.499999999999997,0.707106781186553,0.499999999999996));
#11881=DIRECTION('',(0.707106781186548,0.,0.707106781186548));
#11882=DIRECTION('',(-0.707106781186548,0.,-0.707106781186548));
#11883=DIRECTION('center_axis',(0.,-1.,0.));
#11884=DIRECTION('ref_axis',(-0.923879532511283,0.,-0.382683432365098));
#11885=DIRECTION('',(0.,1.,0.));
#11886=DIRECTION('',(0.,-1.,0.));
#11887=DIRECTION('center_axis',(0.,-1.,0.));
#11888=DIRECTION('ref_axis',(1.,0.,0.));
#11889=DIRECTION('center_axis',(-0.707106781186548,0.,0.707106781186548));
#11890=DIRECTION('ref_axis',(-0.707106781186548,0.,-0.707106781186548));
#11891=DIRECTION('center_axis',(0.,0.,1.));
#11892=DIRECTION('ref_axis',(-1.,0.,0.));
#11893=DIRECTION('center_axis',(-1.,0.,0.));
#11894=DIRECTION('ref_axis',(0.,-1.,0.));
#11895=DIRECTION('center_axis',(0.,0.,1.));
#11896=DIRECTION('ref_axis',(-1.,0.,0.));
#11897=DIRECTION('center_axis',(1.,0.,0.));
#11898=DIRECTION('ref_axis',(0.,0.,1.));
#11899=DIRECTION('center_axis',(1.,0.,0.));
#11900=DIRECTION('ref_axis',(0.,1.,0.));
#11901=DIRECTION('center_axis',(0.,0.,-1.));
#11902=DIRECTION('ref_axis',(1.,0.,0.));
#11903=DIRECTION('center_axis',(0.,0.,1.));
#11904=DIRECTION('ref_axis',(1.,0.,0.));
#11905=DIRECTION('center_axis',(1.,0.,0.));
#11906=DIRECTION('ref_axis',(0.,0.,1.));
#11907=DIRECTION('center_axis',(0.,0.,-1.));
#11908=DIRECTION('ref_axis',(1.,0.,0.));
#11909=DIRECTION('center_axis',(-1.,0.,0.));
#11910=DIRECTION('ref_axis',(0.,0.,-1.));
#11911=DIRECTION('center_axis',(0.,0.,-1.));
#11912=DIRECTION('ref_axis',(1.,0.,0.));
#11913=DIRECTION('center_axis',(0.,1.,0.));
#11914=DIRECTION('ref_axis',(-1.,0.,0.));
#11915=DIRECTION('axis',(0.,0.,1.));
#11916=DIRECTION('refdir',(1.,0.,0.));
#11917=DIRECTION('center_axis',(0.,1.,0.));
#11918=DIRECTION('ref_axis',(1.,0.,0.));
#11919=DIRECTION('center_axis',(-2.22044604925031E-16,-1.,0.));
#11920=DIRECTION('ref_axis',(1.,0.,0.));
#11921=DIRECTION('',(0.,-1.,0.));
#11922=DIRECTION('center_axis',(0.,1.,0.));
#11923=DIRECTION('ref_axis',(1.,0.,0.));
#11924=DIRECTION('center_axis',(0.,-1.,0.));
#11925=DIRECTION('ref_axis',(1.,0.,0.));
#11926=DIRECTION('center_axis',(0.,1.,0.));
#11927=DIRECTION('ref_axis',(1.,0.,0.));
#11928=DIRECTION('center_axis',(-2.22044604925031E-16,-1.,0.));
#11929=DIRECTION('ref_axis',(1.,0.,0.));
#11930=DIRECTION('',(0.,-1.,0.));
#11931=DIRECTION('center_axis',(0.,1.,0.));
#11932=DIRECTION('ref_axis',(1.,0.,0.));
#11933=DIRECTION('center_axis',(0.,-1.,0.));
#11934=DIRECTION('ref_axis',(1.,0.,0.));
#11935=DIRECTION('center_axis',(0.,1.,0.));
#11936=DIRECTION('ref_axis',(1.,0.,0.));
#11937=DIRECTION('center_axis',(-2.22044604925031E-16,-1.,0.));
#11938=DIRECTION('ref_axis',(1.,0.,0.));
#11939=DIRECTION('',(0.,-1.,0.));
#11940=DIRECTION('center_axis',(0.,1.,0.));
#11941=DIRECTION('ref_axis',(1.,0.,0.));
#11942=DIRECTION('center_axis',(0.,-1.,0.));
#11943=DIRECTION('ref_axis',(1.,0.,0.));
#11944=DIRECTION('center_axis',(0.,1.,0.));
#11945=DIRECTION('ref_axis',(1.,0.,0.));
#11946=DIRECTION('center_axis',(-2.22044604925031E-16,-1.,0.));
#11947=DIRECTION('ref_axis',(1.,0.,0.));
#11948=DIRECTION('',(0.,-1.,0.));
#11949=DIRECTION('center_axis',(0.,1.,0.));
#11950=DIRECTION('ref_axis',(1.,0.,0.));
#11951=DIRECTION('center_axis',(0.,-1.,0.));
#11952=DIRECTION('ref_axis',(1.,0.,0.));
#11953=DIRECTION('center_axis',(0.,1.,0.));
#11954=DIRECTION('ref_axis',(1.,0.,0.));
#11955=DIRECTION('center_axis',(2.22044604925031E-16,1.,0.));
#11956=DIRECTION('ref_axis',(1.,0.,0.));
#11957=DIRECTION('',(0.,1.,0.));
#11958=DIRECTION('center_axis',(0.,1.,0.));
#11959=DIRECTION('ref_axis',(1.,0.,0.));
#11960=DIRECTION('center_axis',(0.,-1.,0.));
#11961=DIRECTION('ref_axis',(1.,0.,0.));
#11962=DIRECTION('center_axis',(0.,1.,0.));
#11963=DIRECTION('ref_axis',(1.,0.,0.));
#11964=DIRECTION('center_axis',(2.22044604925031E-16,1.,0.));
#11965=DIRECTION('ref_axis',(1.,0.,0.));
#11966=DIRECTION('',(0.,1.,0.));
#11967=DIRECTION('center_axis',(0.,1.,0.));
#11968=DIRECTION('ref_axis',(1.,0.,0.));
#11969=DIRECTION('center_axis',(0.,-1.,0.));
#11970=DIRECTION('ref_axis',(1.,0.,0.));
#11971=DIRECTION('center_axis',(0.,1.,0.));
#11972=DIRECTION('ref_axis',(1.,0.,0.));
#11973=DIRECTION('center_axis',(2.22044604925031E-16,1.,0.));
#11974=DIRECTION('ref_axis',(1.,0.,0.));
#11975=DIRECTION('',(0.,1.,0.));
#11976=DIRECTION('center_axis',(0.,1.,0.));
#11977=DIRECTION('ref_axis',(1.,0.,0.));
#11978=DIRECTION('center_axis',(0.,-1.,0.));
#11979=DIRECTION('ref_axis',(1.,0.,0.));
#11980=DIRECTION('center_axis',(0.,1.,0.));
#11981=DIRECTION('ref_axis',(1.,0.,0.));
#11982=DIRECTION('center_axis',(2.22044604925031E-16,1.,0.));
#11983=DIRECTION('ref_axis',(1.,0.,0.));
#11984=DIRECTION('',(0.,1.,0.));
#11985=DIRECTION('center_axis',(0.,1.,0.));
#11986=DIRECTION('ref_axis',(1.,0.,0.));
#11987=DIRECTION('center_axis',(0.,-1.,0.));
#11988=DIRECTION('ref_axis',(1.,0.,0.));
#11989=DIRECTION('center_axis',(0.,0.,-1.));
#11990=DIRECTION('ref_axis',(2.22044604925031E-16,1.,0.));
#11991=DIRECTION('center_axis',(0.,0.,1.));
#11992=DIRECTION('ref_axis',(-0.707106781186548,-0.707106781186547,0.));
#11993=DIRECTION('',(-2.22044604925031E-16,-1.,0.));
#11994=DIRECTION('',(1.,-2.22044604925031E-16,0.));
#11995=DIRECTION('',(2.22044604925031E-16,1.,0.));
#11996=DIRECTION('center_axis',(0.,0.,1.));
#11997=DIRECTION('ref_axis',(0.707106781186547,-0.707106781186548,0.));
#11998=DIRECTION('',(1.,-2.22044604925031E-16,0.));
#11999=DIRECTION('center_axis',(0.,0.,1.));
#12000=DIRECTION('ref_axis',(-2.22044604925031E-16,-1.,0.));
#12001=DIRECTION('center_axis',(0.,0.,-1.));
#12002=DIRECTION('ref_axis',(-0.707106781186548,-0.707106781186547,0.));
#12003=DIRECTION('',(-1.,2.22044604925031E-16,0.));
#12004=DIRECTION('center_axis',(0.,0.,-1.));
#12005=DIRECTION('ref_axis',(0.707106781186547,-0.707106781186548,0.));
#12006=DIRECTION('',(-2.22044604925031E-16,-1.,0.));
#12007=DIRECTION('',(1.,-2.22044604925031E-16,0.));
#12008=DIRECTION('',(2.22044604925031E-16,1.,0.));
#12009=DIRECTION('center_axis',(-2.22044604925031E-16,-1.,0.));
#12010=DIRECTION('ref_axis',(0.,0.,-1.));
#12011=DIRECTION('',(0.,0.,-1.));
#12012=DIRECTION('',(0.,0.,1.));
#12013=DIRECTION('center_axis',(0.,0.,1.));
#12014=DIRECTION('ref_axis',(-0.707106781186548,-0.707106781186547,0.));
#12015=DIRECTION('',(0.,0.,-1.));
#12016=DIRECTION('center_axis',(-1.57009245868376E-16,-0.707106781186543,
0.707106781186553));
#12017=DIRECTION('ref_axis',(-1.57009245868379E-16,-0.707106781186553,-0.707106781186543));
#12018=DIRECTION('',(0.,0.,1.));
#12019=DIRECTION('center_axis',(0.,0.,1.));
#12020=DIRECTION('ref_axis',(-0.707106781186548,-0.707106781186547,0.));
#12021=DIRECTION('',(0.,0.,1.));
#12022=DIRECTION('center_axis',(0.,0.,1.));
#12023=DIRECTION('ref_axis',(-2.22044604925031E-16,-1.,0.));
#12024=DIRECTION('',(0.,0.,-1.));
#12025=DIRECTION('center_axis',(-2.22044604925031E-16,-1.,0.));
#12026=DIRECTION('ref_axis',(1.,-2.22044604925031E-16,0.));
#12027=DIRECTION('',(1.,-2.22044604925031E-16,0.));
#12028=DIRECTION('',(0.,0.,-1.));
#12029=DIRECTION('center_axis',(-2.22044604925031E-16,-1.,0.));
#12030=DIRECTION('ref_axis',(1.,-2.22044604925031E-16,0.));
#12031=DIRECTION('',(0.,0.,-1.));
#12032=DIRECTION('',(1.,-2.22044604925031E-16,0.));
#12033=DIRECTION('center_axis',(0.,0.,1.));
#12034=DIRECTION('ref_axis',(0.707106781186547,-0.707106781186548,0.));
#12035=DIRECTION('center_axis',(1.57009245868376E-16,0.707106781186543,
-0.707106781186553));
#12036=DIRECTION('ref_axis',(-1.57009245868379E-16,-0.707106781186553,-0.707106781186542));
#12037=DIRECTION('',(0.,0.,1.));
#12038=DIRECTION('center_axis',(0.,0.,1.));
#12039=DIRECTION('ref_axis',(0.707106781186547,-0.707106781186548,0.));
#12040=DIRECTION('',(0.,0.,1.));
#12041=DIRECTION('center_axis',(0.,0.,1.));
#12042=DIRECTION('ref_axis',(1.,-2.22044604925031E-16,0.));
#12043=DIRECTION('center_axis',(1.,-2.22044604925031E-16,0.));
#12044=DIRECTION('ref_axis',(2.22044604925031E-16,1.,0.));
#12045=DIRECTION('',(-2.22044604925031E-16,-1.,0.));
#12046=DIRECTION('',(0.,0.,-1.));
#12047=DIRECTION('',(-2.22044604925031E-16,-1.,0.));
#12048=DIRECTION('',(0.,0.,1.));
#12049=DIRECTION('',(2.22044604925031E-16,1.,0.));
#12050=DIRECTION('',(0.,0.,-1.));
#12051=DIRECTION('',(2.22044604925031E-16,1.,0.));
#12052=DIRECTION('',(-1.57009245868377E-16,-0.707106781186548,0.707106781186548));
#12053=DIRECTION('center_axis',(1.,-2.22044604925031E-16,0.));
#12054=DIRECTION('ref_axis',(2.05142465794796E-16,0.923879532511307,-0.38268343236504));
#12055=DIRECTION('',(2.22044604925031E-16,1.,0.));
#12056=DIRECTION('',(0.,0.,1.));
#12057=DIRECTION('center_axis',(1.,-2.22044604925031E-16,0.));
#12058=DIRECTION('ref_axis',(1.57009245868378E-16,0.70710678118655,-0.707106781186544));
#12059=DIRECTION('',(2.22044604925031E-16,1.,0.));
#12060=DIRECTION('center_axis',(1.,-2.22044604925031E-16,0.));
#12061=DIRECTION('ref_axis',(-1.57009245868377E-16,-0.707106781186546,-0.707106781186549));
#12062=DIRECTION('',(0.,0.,-1.));
#12063=DIRECTION('',(2.22044604925031E-16,1.,0.));
#12064=DIRECTION('center_axis',(1.,-2.22044604925031E-16,0.));
#12065=DIRECTION('ref_axis',(-1.57009245868377E-16,-0.707106781186546,-0.707106781186549));
#12066=DIRECTION('',(0.,0.,-1.));
#12067=DIRECTION('',(2.22044604925031E-16,1.,0.));
#12068=DIRECTION('center_axis',(0.,0.,1.));
#12069=DIRECTION('ref_axis',(-2.22044604925031E-16,-1.,0.));
#12070=DIRECTION('center_axis',(0.,0.,1.));
#12071=DIRECTION('ref_axis',(0.707106781186548,0.707106781186547,0.));
#12072=DIRECTION('',(1.,-2.22044604925031E-16,0.));
#12073=DIRECTION('',(-2.22044604925031E-16,-1.,0.));
#12074=DIRECTION('center_axis',(0.,0.,1.));
#12075=DIRECTION('ref_axis',(-0.707106781186547,0.707106781186548,0.));
#12076=DIRECTION('',(-1.,2.22044604925031E-16,0.));
#12077=DIRECTION('center_axis',(0.,0.,-1.));
#12078=DIRECTION('ref_axis',(2.22044604925031E-16,1.,0.));
#12079=DIRECTION('center_axis',(0.,0.,-1.));
#12080=DIRECTION('ref_axis',(0.707106781186548,0.707106781186547,0.));
#12081=DIRECTION('',(1.,-2.22044604925031E-16,0.));
#12082=DIRECTION('center_axis',(0.,0.,-1.));
#12083=DIRECTION('ref_axis',(-0.707106781186547,0.707106781186548,0.));
#12084=DIRECTION('',(2.22044604925031E-16,1.,0.));
#12085=DIRECTION('',(1.,-2.22044604925031E-16,0.));
#12086=DIRECTION('center_axis',(-2.22044604925031E-16,-1.,0.));
#12087=DIRECTION('ref_axis',(0.,0.,-1.));
#12088=DIRECTION('',(0.,0.,-1.));
#12089=DIRECTION('center_axis',(0.,0.,1.));
#12090=DIRECTION('ref_axis',(0.707106781186548,0.707106781186547,0.));
#12091=DIRECTION('',(0.,0.,1.));
#12092=DIRECTION('center_axis',(0.,0.,1.));
#12093=DIRECTION('ref_axis',(2.22044604925031E-16,1.,0.));
#12094=DIRECTION('center_axis',(-1.,2.22044604925031E-16,0.));
#12095=DIRECTION('ref_axis',(-2.22044604925031E-16,-1.,0.));
#12096=DIRECTION('',(-2.22044604925031E-16,-1.,0.));
#12097=DIRECTION('',(0.,0.,1.));
#12098=DIRECTION('center_axis',(-1.,2.22044604925031E-16,0.));
#12099=DIRECTION('ref_axis',(-1.57009245868379E-16,-0.707106781186552,-0.707106781186543));
#12100=DIRECTION('',(-2.22044604925031E-16,-1.,0.));
#12101=DIRECTION('',(0.,0.,1.));
#12102=DIRECTION('center_axis',(-1.,2.22044604925031E-16,0.));
#12103=DIRECTION('ref_axis',(-1.57009245868377E-16,-0.707106781186546,-0.707106781186549));
#12104=DIRECTION('',(-2.22044604925031E-16,-1.,0.));
#12105=DIRECTION('center_axis',(-1.,2.22044604925031E-16,0.));
#12106=DIRECTION('ref_axis',(1.57009245868377E-16,0.707106781186547,-0.707106781186547));
#12107=DIRECTION('',(0.,0.,-1.));
#12108=DIRECTION('',(-2.22044604925031E-16,-1.,0.));
#12109=DIRECTION('center_axis',(-1.,2.22044604925031E-16,0.));
#12110=DIRECTION('ref_axis',(2.0514246579479E-16,0.923879532511279,-0.382683432365108));
#12111=DIRECTION('',(1.57009245868377E-16,0.707106781186548,-0.707106781186548));
#12112=DIRECTION('',(-2.22044604925031E-16,-1.,0.));
#12113=DIRECTION('',(0.,0.,1.));
#12114=DIRECTION('',(0.,0.,1.));
#12115=DIRECTION('',(2.22044604925031E-16,1.,0.));
#12116=DIRECTION('center_axis',(2.22044604925031E-16,1.,0.));
#12117=DIRECTION('ref_axis',(-1.,2.22044604925031E-16,0.));
#12118=DIRECTION('',(0.,0.,-1.));
#12119=DIRECTION('',(-1.,2.22044604925031E-16,0.));
#12120=DIRECTION('center_axis',(0.,0.,1.));
#12121=DIRECTION('ref_axis',(-0.707106781186547,0.707106781186548,0.));
#12122=DIRECTION('',(0.,0.,-1.));
#12123=DIRECTION('center_axis',(0.,0.,-1.));
#12124=DIRECTION('ref_axis',(2.22044604925031E-16,1.,0.));
#12125=DIRECTION('center_axis',(1.,-2.22044604925031E-16,0.));
#12126=DIRECTION('ref_axis',(0.,0.,1.));
#12127=DIRECTION('center_axis',(2.22044604925031E-16,1.,0.));
#12128=DIRECTION('ref_axis',(0.,0.,1.));
#12129=DIRECTION('center_axis',(-1.,2.22044604925031E-16,0.));
#12130=DIRECTION('ref_axis',(-2.22044604925031E-16,-1.,0.));
#12131=DIRECTION('center_axis',(0.,0.,1.));
#12132=DIRECTION('ref_axis',(1.,-2.22044604925031E-16,0.));
#12133=DIRECTION('center_axis',(-1.,2.22044604925031E-16,0.));
#12134=DIRECTION('ref_axis',(0.,0.,-1.));
#12135=DIRECTION('center_axis',(0.,0.,1.));
#12136=DIRECTION('ref_axis',(2.22044604925031E-16,1.,0.));
#12137=DIRECTION('center_axis',(1.,-2.22044604925031E-16,0.));
#12138=DIRECTION('ref_axis',(0.,0.,-1.));
#12139=DIRECTION('center_axis',(2.22044604925031E-16,1.,0.));
#12140=DIRECTION('ref_axis',(-1.,2.22044604925031E-16,0.));
#12141=DIRECTION('center_axis',(-0.408248290463861,0.816496580927728,-0.408248290463861));
#12142=DIRECTION('ref_axis',(0.577350269189626,0.577350269189626,0.577350269189626));
#12143=DIRECTION('center_axis',(2.22044604925031E-16,1.,0.));
#12144=DIRECTION('ref_axis',(1.,-2.22044604925031E-16,0.));
#12145=DIRECTION('center_axis',(0.,0.,1.));
#12146=DIRECTION('ref_axis',(2.22044604925031E-16,1.,0.));
#12147=DIRECTION('center_axis',(1.,-2.22044604925031E-16,0.));
#12148=DIRECTION('ref_axis',(0.,0.,1.));
#12149=DIRECTION('center_axis',(-0.408248290463863,0.816496580927726,-0.408248290463863));
#12150=DIRECTION('ref_axis',(0.577350269189626,0.577350269189626,0.577350269189626));
#12151=DIRECTION('center_axis',(2.22044604925031E-16,1.,0.));
#12152=DIRECTION('ref_axis',(1.,-2.22044604925031E-16,0.));
#12153=DIRECTION('center_axis',(4.44089209850056E-15,-9.86076131526251E-31,
1.));
#12154=DIRECTION('ref_axis',(2.22044604925031E-16,1.,0.));
#12155=DIRECTION('center_axis',(1.,-2.22044604925031E-16,0.));
#12156=DIRECTION('ref_axis',(0.,0.,1.));
#12157=DIRECTION('center_axis',(0.,0.,1.));
#12158=DIRECTION('ref_axis',(0.70710678118656,0.707106781186535,0.));
#12159=DIRECTION('',(0.,0.,1.));
#12160=DIRECTION('center_axis',(0.408248290463861,0.816496580927728,-0.408248290463861));
#12161=DIRECTION('ref_axis',(-0.577350269189623,0.577350269189631,0.577350269189623));
#12162=DIRECTION('center_axis',(0.,0.,1.));
#12163=DIRECTION('ref_axis',(-1.,2.22044604925031E-16,0.));
#12164=DIRECTION('center_axis',(2.22044604925031E-16,1.,0.));
#12165=DIRECTION('ref_axis',(0.,0.,1.));
#12166=DIRECTION('center_axis',(-1.,2.22044604925031E-16,0.));
#12167=DIRECTION('ref_axis',(2.22044604925031E-16,1.,0.));
#12168=DIRECTION('center_axis',(2.22044604925031E-16,1.,0.));
#12169=DIRECTION('ref_axis',(-0.707106781186551,1.57009245868378E-16,0.707106781186544));
#12170=DIRECTION('',(2.22044604925031E-16,1.,0.));
#12171=DIRECTION('center_axis',(-1.,2.22044604925031E-16,0.));
#12172=DIRECTION('ref_axis',(1.57009245868377E-16,0.707106781186544,0.707106781186551));
#12173=DIRECTION('',(1.,-2.22044604925031E-16,0.));
#12174=DIRECTION('',(-1.,2.22044604925031E-16,0.));
#12175=DIRECTION('center_axis',(0.408248290463861,0.816496580927736,-0.408248290463846));
#12176=DIRECTION('ref_axis',(-0.577350269189631,0.577350269189616,0.577350269189631));
#12177=DIRECTION('center_axis',(-1.75415237890772E-14,1.,0.));
#12178=DIRECTION('ref_axis',(0.,0.,1.));
#12179=DIRECTION('center_axis',(-1.,2.22044604925031E-16,0.));
#12180=DIRECTION('ref_axis',(2.22044604925031E-16,1.,0.));
#12181=DIRECTION('center_axis',(-9.86076131526251E-31,-4.44089209850056E-15,
1.));
#12182=DIRECTION('ref_axis',(-1.,2.22044604925031E-16,0.));
#12183=DIRECTION('center_axis',(-1.,2.22044604925031E-16,0.));
#12184=DIRECTION('ref_axis',(1.57009245868376E-16,0.707106781186541,0.707106781186554));
#12185=DIRECTION('',(1.,-2.22044604925031E-16,0.));
#12186=DIRECTION('',(-1.,2.22044604925031E-16,0.));
#12187=DIRECTION('center_axis',(0.,0.,-1.));
#12188=DIRECTION('ref_axis',(-0.707106781186547,0.707106781186548,0.));
#12189=DIRECTION('',(0.,0.,-1.));
#12190=DIRECTION('center_axis',(1.,-2.22044604925031E-16,0.));
#12191=DIRECTION('ref_axis',(0.,0.,1.));
#12192=DIRECTION('center_axis',(2.22044604925031E-16,1.,0.));
#12193=DIRECTION('ref_axis',(0.,0.,1.));
#12194=DIRECTION('center_axis',(-1.,2.22044604925031E-16,0.));
#12195=DIRECTION('ref_axis',(-2.22044604925031E-16,-1.,0.));
#12196=DIRECTION('center_axis',(0.,0.,1.));
#12197=DIRECTION('ref_axis',(1.,-2.22044604925031E-16,0.));
#12198=DIRECTION('center_axis',(0.408248290463854,-0.408248290463854,-0.816496580927736));
#12199=DIRECTION('ref_axis',(0.577350269189616,-0.577350269189645,0.577350269189616));
#12200=DIRECTION('center_axis',(1.,-2.22044604925031E-16,0.));
#12201=DIRECTION('ref_axis',(-2.22044604925031E-16,-1.,0.));
#12202=DIRECTION('center_axis',(1.75415237890772E-14,-1.,0.));
#12203=DIRECTION('ref_axis',(0.,0.,1.));
#12204=DIRECTION('center_axis',(-1.,2.22044604925031E-16,0.));
#12205=DIRECTION('ref_axis',(0.,0.,-1.));
#12206=DIRECTION('center_axis',(0.,0.,1.));
#12207=DIRECTION('ref_axis',(2.22044604925031E-16,1.,0.));
#12208=DIRECTION('center_axis',(1.,-2.22044604925031E-16,0.));
#12209=DIRECTION('ref_axis',(0.,0.,-1.));
#12210=DIRECTION('center_axis',(2.22044604925031E-16,1.,0.));
#12211=DIRECTION('ref_axis',(-1.,2.22044604925031E-16,0.));
#12212=DIRECTION('center_axis',(0.,0.,-1.));
#12213=DIRECTION('ref_axis',(-0.707106781186554,0.707106781186541,0.));
#12214=DIRECTION('',(0.,0.,-1.));
#12215=DIRECTION('center_axis',(-1.,2.22044604925031E-16,0.));
#12216=DIRECTION('ref_axis',(-1.57009245868377E-16,-0.707106781186547,-0.707106781186548));
#12217=DIRECTION('',(1.,-2.22044604925031E-16,0.));
#12218=DIRECTION('',(-1.,2.22044604925031E-16,0.));
#12219=DIRECTION('center_axis',(-0.408248290463851,0.816496580927731,0.408248290463865));
#12220=DIRECTION('ref_axis',(-0.577350269189626,-0.577350269189626,0.577350269189626));
#12221=DIRECTION('center_axis',(-2.22044604925031E-16,-1.,0.));
#12222=DIRECTION('ref_axis',(-1.,2.22044604925031E-16,0.));
#12223=DIRECTION('center_axis',(-1.,2.22044604925031E-16,0.));
#12224=DIRECTION('ref_axis',(0.,0.,1.));
#12225=DIRECTION('center_axis',(1.,-2.22044604925031E-16,0.));
#12226=DIRECTION('ref_axis',(0.,0.,1.));
#12227=DIRECTION('center_axis',(0.,0.,1.));
#12228=DIRECTION('ref_axis',(-2.22044604925031E-16,-1.,0.));
#12229=DIRECTION('center_axis',(-1.,2.22044604925031E-16,0.));
#12230=DIRECTION('ref_axis',(0.,0.,-1.));
#12231=DIRECTION('center_axis',(-2.22044604925031E-16,-1.,0.));
#12232=DIRECTION('ref_axis',(1.,-2.22044604925031E-16,0.));
#12233=DIRECTION('center_axis',(-1.,2.22044604925031E-16,0.));
#12234=DIRECTION('ref_axis',(0.,0.,-1.));
#12235=DIRECTION('center_axis',(-2.22044604925031E-16,-1.,0.));
#12236=DIRECTION('ref_axis',(0.,0.,1.));
#12237=DIRECTION('center_axis',(1.,-2.22044604925031E-16,0.));
#12238=DIRECTION('ref_axis',(2.22044604925031E-16,1.,0.));
#12239=DIRECTION('center_axis',(0.,0.,1.));
#12240=DIRECTION('ref_axis',(-1.,2.22044604925031E-16,0.));
#12241=DIRECTION('center_axis',(2.22044604925031E-16,1.,0.));
#12242=DIRECTION('ref_axis',(-0.707106781186553,1.57009245868379E-16,0.707106781186542));
#12243=DIRECTION('',(2.22044604925031E-16,1.,0.));
#12244=DIRECTION('center_axis',(-1.,2.22044604925031E-16,0.));
#12245=DIRECTION('ref_axis',(1.57009245868377E-16,0.707106781186546,-0.707106781186549));
#12246=DIRECTION('',(1.,-2.22044604925031E-16,0.));
#12247=DIRECTION('',(-1.,2.22044604925031E-16,0.));
#12248=DIRECTION('center_axis',(0.408248290463858,0.816496580927738,0.408248290463844));
#12249=DIRECTION('ref_axis',(0.577350269189642,-0.577350269189607,0.577350269189628));
#12250=DIRECTION('center_axis',(0.,0.,1.));
#12251=DIRECTION('ref_axis',(1.,-2.22044604925031E-16,0.));
#12252=DIRECTION('center_axis',(1.75415237890772E-14,-1.,0.));
#12253=DIRECTION('ref_axis',(0.,0.,1.));
#12254=DIRECTION('center_axis',(1.,-2.22044604925031E-16,0.));
#12255=DIRECTION('ref_axis',(-2.22044604925031E-16,-1.,0.));
#12256=DIRECTION('center_axis',(-0.408248290463858,-0.408248290463858,-0.816496580927731));
#12257=DIRECTION('ref_axis',(0.577350269189626,0.577350269189626,-0.577350269189626));
#12258=DIRECTION('center_axis',(0.,0.,-1.));
#12259=DIRECTION('ref_axis',(1.,-2.22044604925031E-16,0.));
#12260=DIRECTION('center_axis',(2.22044604925031E-16,1.,0.));
#12261=DIRECTION('ref_axis',(0.,0.,-1.));
#12262=DIRECTION('center_axis',(1.,-2.22044604925031E-16,0.));
#12263=DIRECTION('ref_axis',(2.22044604925031E-16,1.,0.));
#12264=DIRECTION('center_axis',(2.22044604925031E-16,1.,0.));
#12265=DIRECTION('ref_axis',(0.707106781186553,-1.57009245868379E-16,-0.707106781186543));
#12266=DIRECTION('',(2.22044604925031E-16,1.,0.));
#12267=DIRECTION('center_axis',(-0.408248290463861,0.816496580927728,0.408248290463861));
#12268=DIRECTION('ref_axis',(-0.577350269189623,-0.577350269189631,0.577350269189623));
#12269=DIRECTION('center_axis',(-2.22044604925031E-16,-1.,-8.88178419700124E-15));
#12270=DIRECTION('ref_axis',(-1.,2.22044604925031E-16,0.));
#12271=DIRECTION('center_axis',(0.,0.,1.));
#12272=DIRECTION('ref_axis',(-2.22044604925031E-16,-1.,0.));
#12273=DIRECTION('center_axis',(-1.,2.22044604925031E-16,0.));
#12274=DIRECTION('ref_axis',(0.,0.,1.));
#12275=DIRECTION('center_axis',(0.,0.,1.));
#12276=DIRECTION('ref_axis',(-0.707106781186554,-0.707106781186541,0.));
#12277=DIRECTION('',(0.,0.,1.));
#12278=DIRECTION('center_axis',(-1.,2.22044604925031E-16,0.));
#12279=DIRECTION('ref_axis',(-1.57009245868377E-16,-0.707106781186544,0.707106781186551));
#12280=DIRECTION('',(1.,-2.22044604925031E-16,0.));
#12281=DIRECTION('',(-1.,2.22044604925031E-16,0.));
#12282=DIRECTION('center_axis',(0.408248290463856,0.81649658092774,0.408248290463842));
#12283=DIRECTION('ref_axis',(-0.577350269189626,0.577350269189626,-0.577350269189626));
#12284=DIRECTION('center_axis',(-1.,2.22044604925031E-16,0.));
#12285=DIRECTION('ref_axis',(0.,0.,-1.));
#12286=DIRECTION('center_axis',(2.22044604925031E-16,1.,1.77635683940025E-14));
#12287=DIRECTION('ref_axis',(-1.,2.22044604925031E-16,0.));
#12288=DIRECTION('center_axis',(-1.,2.22044604925031E-16,0.));
#12289=DIRECTION('ref_axis',(1.57009245868376E-16,0.70710678118654,-0.707106781186555));
#12290=DIRECTION('',(1.,-2.22044604925031E-16,0.));
#12291=DIRECTION('',(-1.,2.22044604925031E-16,0.));
#12292=DIRECTION('center_axis',(-2.22044604925031E-16,-1.,0.));
#12293=DIRECTION('ref_axis',(-0.707106781186553,1.57009245868379E-16,-0.707106781186543));
#12294=DIRECTION('',(-2.22044604925031E-16,-1.,0.));
#12295=DIRECTION('center_axis',(1.,-2.22044604925031E-16,-3.55271367880045E-14));
#12296=DIRECTION('ref_axis',(2.8421709430404E-14,0.,1.));
#12297=DIRECTION('center_axis',(2.49644700930717E-14,-0.707106781186548,
0.707106781186548));
#12298=DIRECTION('ref_axis',(-1.57009245868377E-16,-0.707106781186548,-0.707106781186548));
#12299=DIRECTION('center_axis',(-1.,2.22044604925031E-16,0.));
#12300=DIRECTION('ref_axis',(0.,0.,-1.));
#12301=DIRECTION('center_axis',(-2.22044604925031E-16,-1.,0.));
#12302=DIRECTION('ref_axis',(1.,-2.22044604925031E-16,0.));
#12303=DIRECTION('center_axis',(-0.408248290463851,0.816496580927731,-0.408248290463865));
#12304=DIRECTION('ref_axis',(0.577350269189626,0.577350269189626,0.577350269189626));
#12305=DIRECTION('center_axis',(2.22044604925031E-16,1.,0.));
#12306=DIRECTION('ref_axis',(1.,-2.22044604925031E-16,0.));
#12307=DIRECTION('center_axis',(1.,-2.22044604925031E-16,0.));
#12308=DIRECTION('ref_axis',(0.,0.,1.));
#12309=DIRECTION('center_axis',(0.,0.,1.));
#12310=DIRECTION('ref_axis',(0.707106781186548,0.707106781186547,0.));
#12311=DIRECTION('',(0.,0.,1.));
#12312=DIRECTION('center_axis',(1.,-2.22044604925031E-16,0.));
#12313=DIRECTION('ref_axis',(0.,0.,1.));
#12314=DIRECTION('center_axis',(-2.22044604925031E-16,-1.,0.));
#12315=DIRECTION('ref_axis',(0.,0.,1.));
#12316=DIRECTION('center_axis',(1.,-2.22044604925031E-16,0.));
#12317=DIRECTION('ref_axis',(1.57009245868377E-16,0.707106781186548,0.707106781186548));
#12318=DIRECTION('center_axis',(-1.57009245868379E-16,-0.707106781186554,
0.707106781186541));
#12319=DIRECTION('ref_axis',(-1.,2.22044604925031E-16,0.));
#12320=DIRECTION('center_axis',(-0.408248290463854,0.408248290463854,-0.816496580927736));
#12321=DIRECTION('ref_axis',(-0.577350269189616,0.577350269189645,0.577350269189616));
#12322=DIRECTION('center_axis',(-1.,2.22044604925031E-16,0.));
#12323=DIRECTION('ref_axis',(2.22044604925031E-16,1.,0.));
#12324=DIRECTION('center_axis',(0.,0.,1.));
#12325=DIRECTION('ref_axis',(-1.,2.22044604925031E-16,0.));
#12326=DIRECTION('center_axis',(-1.75415237890772E-14,1.,0.));
#12327=DIRECTION('ref_axis',(0.,0.,1.));
#12328=DIRECTION('center_axis',(0.,0.,1.));
#12329=DIRECTION('ref_axis',(-0.707106781186547,0.707106781186548,0.));
#12330=DIRECTION('center_axis',(0.538877990790914,0.827465426020369,0.157833709270475));
#12331=DIRECTION('ref_axis',(0.794104487760817,-0.561516668266341,0.232587819494483));
#12332=DIRECTION('center_axis',(1.,-2.22044604925031E-16,0.));
#12333=DIRECTION('ref_axis',(-1.57009245868377E-16,-0.707106781186548,-0.707106781186548));
#12334=DIRECTION('center_axis',(-1.57009245868377E-16,-0.707106781186548,
0.707106781186548));
#12335=DIRECTION('ref_axis',(1.,-2.22044604925031E-16,0.));
#12336=DIRECTION('center_axis',(-2.22044604925031E-16,-1.,0.));
#12337=DIRECTION('ref_axis',(0.,0.,1.));
#12338=DIRECTION('center_axis',(1.57009245868377E-16,0.707106781186548,
-0.707106781186548));
#12339=DIRECTION('ref_axis',(0.707106781186553,-0.499999999999996,-0.499999999999996));
#12340=DIRECTION('',(1.57009245868377E-16,0.707106781186548,-0.707106781186548));
#12341=DIRECTION('center_axis',(2.22044604925031E-16,1.,0.));
#12342=DIRECTION('ref_axis',(0.707106781186551,-1.57009245868378E-16,0.707106781186544));
#12343=DIRECTION('',(-2.22044604925031E-16,-1.,0.));
#12344=DIRECTION('center_axis',(-0.53887799079092,0.827465426020364,0.157833709270477));
#12345=DIRECTION('ref_axis',(-0.794104487760823,-0.561516668266338,0.23258781949447));
#12346=DIRECTION('center_axis',(-1.57009245868377E-16,-0.707106781186548,
0.707106781186548));
#12347=DIRECTION('ref_axis',(-1.57009245868377E-16,-0.707106781186548,-0.707106781186548));
#12348=DIRECTION('center_axis',(-1.,2.22044604925031E-16,0.));
#12349=DIRECTION('ref_axis',(0.,0.,1.));
#12350=DIRECTION('center_axis',(-2.22044604925031E-16,-1.,0.));
#12351=DIRECTION('ref_axis',(-1.,2.22044604925031E-16,0.));
#12352=DIRECTION('center_axis',(1.,-2.22044604925031E-16,0.));
#12353=DIRECTION('ref_axis',(-2.05142465794791E-16,-0.923879532511288,0.382683432365088));
#12354=DIRECTION('',(-1.,2.22044604925031E-16,0.));
#12355=DIRECTION('',(1.,-2.22044604925031E-16,0.));
#12356=DIRECTION('center_axis',(-2.22044604925031E-16,-1.,0.));
#12357=DIRECTION('ref_axis',(-0.707106781186551,1.57009245868378E-16,0.707106781186544));
#12358=DIRECTION('',(2.22044604925031E-16,1.,0.));
#12359=DIRECTION('center_axis',(-1.57009245868377E-16,-0.707106781186548,
0.707106781186548));
#12360=DIRECTION('ref_axis',(-0.707106781186553,-0.499999999999996,-0.499999999999996));
#12361=DIRECTION('',(-1.57009245868377E-16,-0.707106781186548,0.707106781186548));
#12362=DIRECTION('center_axis',(-1.,2.22044604925031E-16,0.));
#12363=DIRECTION('ref_axis',(1.57009245868375E-16,0.707106781186538,0.707106781186557));
#12364=DIRECTION('',(1.,-2.22044604925031E-16,0.));
#12365=DIRECTION('center_axis',(2.22044604925031E-16,1.,0.));
#12366=DIRECTION('ref_axis',(-0.707106781186551,1.57009245868378E-16,0.707106781186544));
#12367=DIRECTION('',(2.22044604925031E-16,1.,0.));
#12368=DIRECTION('center_axis',(-1.,2.22044604925031E-16,0.));
#12369=DIRECTION('ref_axis',(2.05142465794791E-16,0.923879532511288,-0.382683432365088));
#12370=DIRECTION('',(1.,-2.22044604925031E-16,0.));
#12371=DIRECTION('',(-1.,2.22044604925031E-16,0.));
#12372=DIRECTION('center_axis',(-2.22044604925031E-16,-1.,0.));
#12373=DIRECTION('ref_axis',(0.707106781186551,-1.57009245868378E-16,0.707106781186544));
#12374=DIRECTION('',(-2.22044604925031E-16,-1.,0.));
#12375=DIRECTION('center_axis',(0.,0.,-1.));
#12376=DIRECTION('ref_axis',(0.707106781186547,-0.707106781186548,0.));
#12377=DIRECTION('',(0.,0.,-1.));
#12378=DIRECTION('center_axis',(-2.22044604925031E-16,-1.,0.));
#12379=DIRECTION('ref_axis',(0.707106781186553,-1.57009245868379E-16,0.707106781186542));
#12380=DIRECTION('',(-2.22044604925031E-16,-1.,0.));
#12381=DIRECTION('center_axis',(1.,-2.22044604925031E-16,0.));
#12382=DIRECTION('ref_axis',(-1.57009245868375E-16,-0.707106781186538,0.707106781186557));
#12383=DIRECTION('',(-1.,2.22044604925031E-16,0.));
#12384=DIRECTION('center_axis',(-2.22044604925031E-16,-1.,0.));
#12385=DIRECTION('ref_axis',(-0.707106781186551,1.57009245868378E-16,0.707106781186544));
#12386=DIRECTION('',(2.22044604925031E-16,1.,0.));
#12387=DIRECTION('center_axis',(2.22044604925031E-16,1.,0.));
#12388=DIRECTION('ref_axis',(0.707106781186551,-1.57009245868378E-16,0.707106781186544));
#12389=DIRECTION('',(-2.22044604925031E-16,-1.,0.));
#12390=DIRECTION('center_axis',(0.,0.,1.));
#12391=DIRECTION('ref_axis',(0.707106781186554,0.707106781186541,0.));
#12392=DIRECTION('',(0.,0.,1.));
#12393=DIRECTION('center_axis',(-2.22044604925031E-16,-1.,0.));
#12394=DIRECTION('ref_axis',(0.707106781186551,-1.57009245868378E-16,0.707106781186544));
#12395=DIRECTION('',(-2.22044604925031E-16,-1.,0.));
#12396=DIRECTION('center_axis',(-1.,2.22044604925031E-16,0.));
#12397=DIRECTION('ref_axis',(-1.57009245868375E-16,-0.707106781186538,-0.707106781186557));
#12398=DIRECTION('',(1.,-2.22044604925031E-16,0.));
#12399=DIRECTION('',(-1.,2.22044604925031E-16,0.));
#12400=DIRECTION('center_axis',(0.,0.,1.));
#12401=DIRECTION('ref_axis',(-2.22044604925031E-16,-1.,0.));
#12402=DIRECTION('center_axis',(-2.22044604925031E-16,-1.,0.));
#12403=DIRECTION('ref_axis',(0.,0.,1.));
#12404=DIRECTION('center_axis',(0.,0.,-1.));
#12405=DIRECTION('ref_axis',(-2.22044604925031E-16,-1.,0.));
#12406=DIRECTION('center_axis',(-2.22044604925031E-16,-1.,0.));
#12407=DIRECTION('ref_axis',(0.,0.,1.));
#12408=DIRECTION('center_axis',(0.,0.,-1.));
#12409=DIRECTION('ref_axis',(-2.22044604925031E-16,-1.,0.));
#12410=DIRECTION('center_axis',(2.22044604925031E-16,1.,0.));
#12411=DIRECTION('ref_axis',(0.,0.,-1.));
#12412=DIRECTION('center_axis',(0.,0.,-1.));
#12413=DIRECTION('ref_axis',(-2.22044604925031E-16,-1.,0.));
#12414=DIRECTION('center_axis',(2.22044604925031E-16,1.,0.));
#12415=DIRECTION('ref_axis',(-1.,2.22044604925031E-16,0.));
#12416=DIRECTION('center_axis',(1.57009245868377E-16,0.707106781186548,
0.707106781186548));
#12417=DIRECTION('ref_axis',(1.57009245868377E-16,0.707106781186548,-0.707106781186548));
#12418=DIRECTION('center_axis',(0.,0.,1.));
#12419=DIRECTION('ref_axis',(-2.22044604925031E-16,-1.,0.));
#12420=DIRECTION('center_axis',(0.,0.,1.));
#12421=DIRECTION('ref_axis',(-2.22044604925031E-16,-1.,0.));
#12422=DIRECTION('axis',(0.,0.,1.));
#12423=DIRECTION('refdir',(1.,0.,0.));
#12424=DIRECTION('center_axis',(-1.,0.,0.));
#12425=DIRECTION('ref_axis',(0.,-0.707106781186519,-0.707106781186576));
#12426=DIRECTION('center_axis',(-1.,0.,0.));
#12427=DIRECTION('ref_axis',(0.,0.,-1.));
#12428=DIRECTION('',(-1.,0.,0.));
#12429=DIRECTION('center_axis',(1.,0.,0.));
#12430=DIRECTION('ref_axis',(0.,-1.,0.));
#12431=DIRECTION('',(1.,0.,0.));
#12432=DIRECTION('center_axis',(0.,0.,1.));
#12433=DIRECTION('ref_axis',(1.,0.,0.));
#12434=DIRECTION('center_axis',(-1.,0.,0.));
#12435=DIRECTION('ref_axis',(0.,1.,0.));
#12436=DIRECTION('center_axis',(0.,0.,-1.));
#12437=DIRECTION('ref_axis',(1.,0.,0.));
#12438=DIRECTION('center_axis',(0.,0.,1.));
#12439=DIRECTION('ref_axis',(1.,0.,0.));
#12440=DIRECTION('center_axis',(1.,0.,0.));
#12441=DIRECTION('ref_axis',(0.,0.707106781186561,-0.707106781186534));
#12442=DIRECTION('center_axis',(-1.,0.,0.));
#12443=DIRECTION('ref_axis',(0.,1.,0.));
#12444=DIRECTION('',(-1.,0.,0.));
#12445=DIRECTION('',(1.,0.,0.));
#12446=DIRECTION('center_axis',(0.,0.,1.));
#12447=DIRECTION('ref_axis',(-1.,0.,0.));
#12448=DIRECTION('center_axis',(0.,0.,-1.));
#12449=DIRECTION('ref_axis',(-1.,0.,0.));
#12450=DIRECTION('center_axis',(0.,0.,1.));
#12451=DIRECTION('ref_axis',(-1.,0.,0.));
#12452=DIRECTION('center_axis',(0.,0.,1.));
#12453=DIRECTION('ref_axis',(0.,1.,0.));
#12454=DIRECTION('',(0.,0.,-1.));
#12455=DIRECTION('center_axis',(0.,0.,1.));
#12456=DIRECTION('ref_axis',(1.,0.,0.));
#12457=DIRECTION('',(0.,0.,-1.));
#12458=DIRECTION('center_axis',(0.,-1.,0.));
#12459=DIRECTION('ref_axis',(-1.,0.,0.));
#12460=DIRECTION('',(-1.,0.,0.));
#12461=DIRECTION('',(0.,0.,-1.));
#12462=DIRECTION('center_axis',(0.,0.,1.));
#12463=DIRECTION('ref_axis',(-1.,0.,0.));
#12464=DIRECTION('',(1.,0.,0.));
#12465=DIRECTION('',(0.,-1.,0.));
#12466=DIRECTION('',(-1.,0.,0.));
#12467=DIRECTION('',(0.,1.,0.));
#12468=DIRECTION('center_axis',(0.,1.,0.));
#12469=DIRECTION('ref_axis',(0.,0.,-1.));
#12470=DIRECTION('center_axis',(-1.,0.,0.));
#12471=DIRECTION('ref_axis',(0.,0.,-1.));
#12472=DIRECTION('center_axis',(0.,1.,0.));
#12473=DIRECTION('ref_axis',(-0.70710678118654,0.,0.707106781186555));
#12474=DIRECTION('center_axis',(0.,0.,1.));
#12475=DIRECTION('ref_axis',(0.,-1.,0.));
#12476=DIRECTION('center_axis',(0.,-1.,0.));
#12477=DIRECTION('ref_axis',(-1.,0.,0.));
#12478=DIRECTION('center_axis',(-0.816496580927734,0.408248290463867,0.408248290463843));
#12479=DIRECTION('ref_axis',(-0.577350269189598,-0.577350269189645,-0.577350269189634));
#12480=DIRECTION('center_axis',(1.,0.,0.));
#12481=DIRECTION('ref_axis',(0.,0.,-1.));
#12482=DIRECTION('center_axis',(9.25185853854317E-16,0.,1.));
#12483=DIRECTION('ref_axis',(0.,-1.,0.));
#12484=DIRECTION('center_axis',(0.,1.,0.));
#12485=DIRECTION('ref_axis',(-1.,0.,0.));
#12486=DIRECTION('center_axis',(0.,1.,0.));
#12487=DIRECTION('ref_axis',(0.,0.,-1.));
#12488=DIRECTION('center_axis',(0.,-1.,0.));
#12489=DIRECTION('ref_axis',(-0.70710678118654,0.,0.707106781186555));
#12490=DIRECTION('center_axis',(-1.,0.,0.));
#12491=DIRECTION('ref_axis',(0.,1.,0.));
#12492=DIRECTION('center_axis',(5.92118946466763E-14,1.,0.));
#12493=DIRECTION('ref_axis',(0.,0.,1.));
#12494=DIRECTION('center_axis',(0.,0.,1.));
#12495=DIRECTION('ref_axis',(1.,0.,0.));
#12496=DIRECTION('center_axis',(0.,0.,1.));
#12497=DIRECTION('ref_axis',(0.707106781186547,0.707106781186547,0.));
#12498=DIRECTION('',(0.,0.,1.));
#12499=DIRECTION('center_axis',(-0.707106781186576,0.,-0.707106781186519));
#12500=DIRECTION('ref_axis',(-0.707106781186519,0.,0.707106781186576));
#12501=DIRECTION('',(0.,0.,-1.));
#12502=DIRECTION('center_axis',(-0.827465426020362,-0.538877990790925,-0.157833709270471));
#12503=DIRECTION('ref_axis',(0.561516668266355,-0.794104487760816,-0.232587819494453));
#12504=DIRECTION('center_axis',(-0.707106781186544,-3.663549070262E-14,
0.707106781186551));
#12505=DIRECTION('ref_axis',(0.707106781186551,0.,0.707106781186544));
#12506=DIRECTION('center_axis',(-1.,0.,2.96059473233375E-14));
#12507=DIRECTION('ref_axis',(0.,-1.,0.));
#12508=DIRECTION('center_axis',(0.,1.,0.));
#12509=DIRECTION('ref_axis',(0.,0.,-1.));
#12510=DIRECTION('center_axis',(0.408248290463871,-0.408248290463824,-0.816496580927742));
#12511=DIRECTION('ref_axis',(-0.577350269189681,0.577350269189586,-0.57735026918961));
#12512=DIRECTION('center_axis',(0.,-1.,0.));
#12513=DIRECTION('ref_axis',(0.,0.,-1.));
#12514=DIRECTION('center_axis',(0.,-9.25185853854317E-16,1.));
#12515=DIRECTION('ref_axis',(-1.,0.,0.));
#12516=DIRECTION('center_axis',(1.,0.,-5.9211894646675E-14));
#12517=DIRECTION('ref_axis',(0.,1.,0.));
#12518=DIRECTION('center_axis',(1.,0.,0.));
#12519=DIRECTION('ref_axis',(0.,0.707106781186519,-0.707106781186576));
#12520=DIRECTION('',(-1.,0.,0.));
#12521=DIRECTION('',(1.,0.,0.));
#12522=DIRECTION('center_axis',(-0.408248290463859,-0.408248290463835,-0.816496580927742));
#12523=DIRECTION('ref_axis',(-0.577350269189665,-0.577350269189618,0.577350269189594));
#12524=DIRECTION('center_axis',(0.,0.,-1.));
#12525=DIRECTION('ref_axis',(-1.,0.,0.));
#12526=DIRECTION('center_axis',(1.,0.,-5.9211894646675E-14));
#12527=DIRECTION('ref_axis',(0.,-1.,0.));
#12528=DIRECTION('center_axis',(0.,1.,0.));
#12529=DIRECTION('ref_axis',(0.,0.,1.));
#12530=DIRECTION('center_axis',(-0.827465426020388,0.538877990790895,-0.157833709270442));
#12531=DIRECTION('ref_axis',(0.561516668266318,0.794104487760845,-0.232587819494444));
#12532=DIRECTION('center_axis',(0.,-1.,0.));
#12533=DIRECTION('ref_axis',(0.707106781186544,0.,0.707106781186551));
#12534=DIRECTION('center_axis',(-1.,2.96059473233364E-14,0.));
#12535=DIRECTION('ref_axis',(0.,0.,-1.));
#12536=DIRECTION('center_axis',(-0.70710678118657,0.,0.707106781186525));
#12537=DIRECTION('ref_axis',(0.,1.,0.));
#12538=DIRECTION('center_axis',(0.182143211721521,0.879465224064606,0.439732612032315));
#12539=DIRECTION('ref_axis',(0.336556770590777,-0.475963149477983,0.812519920068737));
#12540=DIRECTION('center_axis',(-1.,0.,0.));
#12541=DIRECTION('ref_axis',(0.,0.,1.));
#12542=DIRECTION('center_axis',(0.70710678118654,0.,-0.707106781186555));
#12543=DIRECTION('ref_axis',(0.,-1.,0.));
#12544=DIRECTION('center_axis',(0.,1.,0.));
#12545=DIRECTION('ref_axis',(0.707106781186551,0.,0.707106781186544));
#12546=DIRECTION('center_axis',(-0.408248290463908,0.408248290463861,-0.816496580927704));
#12547=DIRECTION('ref_axis',(-0.577350269189642,0.577350269189594,0.577350269189642));
#12548=DIRECTION('center_axis',(0.,-1.,-5.9211894646675E-14));
#12549=DIRECTION('ref_axis',(-1.,0.,0.));
#12550=DIRECTION('center_axis',(1.,0.,0.));
#12551=DIRECTION('ref_axis',(0.,0.,1.));
#12552=DIRECTION('center_axis',(0.,0.,-1.));
#12553=DIRECTION('ref_axis',(0.,1.,0.));
#12554=DIRECTION('center_axis',(0.,0.,-1.));
#12555=DIRECTION('ref_axis',(-0.707106781186589,0.707106781186506,0.));
#12556=DIRECTION('',(0.,0.,1.));
#12557=DIRECTION('',(0.,0.,-1.));
#12558=DIRECTION('center_axis',(-0.182143211721517,0.879465224064606,-0.439732612032315));
#12559=DIRECTION('ref_axis',(0.336556770590767,0.475963149477992,0.812519920068736));
#12560=DIRECTION('center_axis',(0.,-1.,0.));
#12561=DIRECTION('ref_axis',(0.,0.,1.));
#12562=DIRECTION('center_axis',(0.70710678118654,0.,-0.707106781186555));
#12563=DIRECTION('ref_axis',(0.707106781186555,0.,0.70710678118654));
#12564=DIRECTION('center_axis',(-1.,0.,0.));
#12565=DIRECTION('ref_axis',(0.,1.,0.));
#12566=DIRECTION('center_axis',(1.,0.,0.));
#12567=DIRECTION('ref_axis',(0.,0.707106781186558,0.707106781186537));
#12568=DIRECTION('',(-1.,0.,0.));
#12569=DIRECTION('',(1.,0.,0.));
#12570=DIRECTION('center_axis',(0.707106781186547,0.,-0.707106781186548));
#12571=DIRECTION('ref_axis',(0.499999999999997,0.707106781186559,0.499999999999986));
#12572=DIRECTION('',(-0.707106781186547,0.,0.707106781186548));
#12573=DIRECTION('',(0.707106781186547,0.,-0.707106781186548));
#12574=DIRECTION('center_axis',(0.,1.,0.));
#12575=DIRECTION('ref_axis',(0.382683432365094,0.,0.923879532511285));
#12576=DIRECTION('',(0.,-1.,0.));
#12577=DIRECTION('',(0.,1.,0.));
#12578=DIRECTION('center_axis',(0.,1.,0.));
#12579=DIRECTION('ref_axis',(-0.707106781186558,0.,0.707106781186537));
#12580=DIRECTION('',(0.,-1.,0.));
#12581=DIRECTION('',(0.,1.,0.));
#12582=DIRECTION('center_axis',(-0.707106781186547,0.,0.707106781186548));
#12583=DIRECTION('ref_axis',(0.499999999999997,-0.707106781186559,0.499999999999986));
#12584=DIRECTION('',(0.707106781186547,0.,-0.707106781186548));
#12585=DIRECTION('',(-0.707106781186547,0.,0.707106781186548));
#12586=DIRECTION('center_axis',(-1.,0.,0.));
#12587=DIRECTION('ref_axis',(0.,-0.707106781186558,0.707106781186537));
#12588=DIRECTION('',(1.,0.,0.));
#12589=DIRECTION('',(-1.,0.,0.));
#12590=DIRECTION('center_axis',(-1.,0.,0.));
#12591=DIRECTION('ref_axis',(0.,0.707106781186561,-0.707106781186534));
#12592=DIRECTION('',(-1.,0.,0.));
#12593=DIRECTION('center_axis',(0.,1.,0.));
#12594=DIRECTION('ref_axis',(0.923879532511297,0.,-0.382683432365066));
#12595=DIRECTION('',(0.,1.,0.));
#12596=DIRECTION('center_axis',(0.,0.,-1.));
#12597=DIRECTION('ref_axis',(-0.707106781186506,-0.707106781186589,0.));
#12598=DIRECTION('',(0.,0.,1.));
#12599=DIRECTION('',(0.,0.,-1.));
#12600=DIRECTION('center_axis',(0.,1.,0.));
#12601=DIRECTION('ref_axis',(-0.707106781186519,0.,-0.707106781186576));
#12602=DIRECTION('',(0.,-1.,0.));
#12603=DIRECTION('',(0.,1.,0.));
#12604=DIRECTION('center_axis',(1.,0.,0.));
#12605=DIRECTION('ref_axis',(0.,-0.707106781186561,-0.707106781186534));
#12606=DIRECTION('',(1.,0.,0.));
#12607=DIRECTION('center_axis',(0.,1.,0.));
#12608=DIRECTION('ref_axis',(-0.707106781186519,0.,0.707106781186576));
#12609=DIRECTION('',(0.,-1.,0.));
#12610=DIRECTION('center_axis',(1.,0.,0.));
#12611=DIRECTION('ref_axis',(0.,-0.707106781186561,-0.707106781186534));
#12612=DIRECTION('',(-1.,0.,0.));
#12613=DIRECTION('center_axis',(0.707106781186555,0.,0.70710678118654));
#12614=DIRECTION('ref_axis',(0.70710678118654,0.,-0.707106781186555));
#12615=DIRECTION('',(1.,0.,0.));
#12616=DIRECTION('center_axis',(0.,0.,1.));
#12617=DIRECTION('ref_axis',(0.707106781186506,-0.707106781186589,0.));
#12618=DIRECTION('',(0.,0.,1.));
#12619=DIRECTION('',(0.,0.,-1.));
#12620=DIRECTION('center_axis',(-1.,0.,0.));
#12621=DIRECTION('ref_axis',(0.,0.,-1.));
#12622=DIRECTION('',(0.,-1.,0.));
#12623=DIRECTION('center_axis',(0.,1.,0.));
#12624=DIRECTION('ref_axis',(1.,0.,0.));
#12625=DIRECTION('center_axis',(1.,0.,0.));
#12626=DIRECTION('ref_axis',(0.,0.,1.));
#12627=DIRECTION('center_axis',(0.,0.,-1.));
#12628=DIRECTION('ref_axis',(1.,0.,0.));
#12629=DIRECTION('',(1.,0.,0.));
#12630=DIRECTION('center_axis',(0.,0.,-1.));
#12631=DIRECTION('ref_axis',(1.,0.,0.));
#12632=DIRECTION('',(-1.,0.,0.));
#12633=DIRECTION('center_axis',(0.,0.,-1.));
#12634=DIRECTION('ref_axis',(-1.,0.,0.));
#12635=DIRECTION('center_axis',(-0.707106781186548,0.,-0.707106781186547));
#12636=DIRECTION('ref_axis',(0.707106781186547,0.,-0.707106781186548));
#12637=DIRECTION('center_axis',(0.,1.,0.));
#12638=DIRECTION('ref_axis',(0.,0.,1.));
#12639=DIRECTION('center_axis',(1.,0.,0.));
#12640=DIRECTION('ref_axis',(0.,-0.707106781186516,0.707106781186579));
#12641=DIRECTION('center_axis',(1.,0.,0.));
#12642=DIRECTION('ref_axis',(0.,0.,1.));
#12643=DIRECTION('center_axis',(-1.,0.,0.));
#12644=DIRECTION('ref_axis',(0.,-1.,0.));
#12645=DIRECTION('center_axis',(0.,0.,-1.));
#12646=DIRECTION('ref_axis',(-1.,0.,0.));
#12647=DIRECTION('center_axis',(1.,0.,0.));
#12648=DIRECTION('ref_axis',(0.,1.,0.));
#12649=DIRECTION('center_axis',(0.,0.,1.));
#12650=DIRECTION('ref_axis',(-1.,0.,0.));
#12651=DIRECTION('center_axis',(-1.,0.,0.));
#12652=DIRECTION('ref_axis',(0.,0.707106781186558,0.707106781186537));
#12653=DIRECTION('center_axis',(1.,0.,0.));
#12654=DIRECTION('ref_axis',(0.,1.,0.));
#12655=DIRECTION('',(1.,0.,0.));
#12656=DIRECTION('center_axis',(0.,0.,-1.));
#12657=DIRECTION('ref_axis',(1.,0.,0.));
#12658=DIRECTION('center_axis',(0.,0.,1.));
#12659=DIRECTION('ref_axis',(0.,-1.,0.));
#12660=DIRECTION('',(0.,0.,-1.));
#12661=DIRECTION('center_axis',(0.,1.,0.));
#12662=DIRECTION('ref_axis',(1.,0.,0.));
#12663=DIRECTION('center_axis',(0.,0.,1.));
#12664=DIRECTION('ref_axis',(-1.,0.,0.));
#12665=DIRECTION('axis',(0.,0.,1.));
#12666=DIRECTION('refdir',(1.,0.,0.));
#12667=DIRECTION('center_axis',(0.,0.,-1.));
#12668=DIRECTION('ref_axis',(-1.,0.,0.));
#12669=DIRECTION('center_axis',(0.,0.,-1.));
#12670=DIRECTION('ref_axis',(-1.,0.,0.));
#12671=DIRECTION('',(0.,0.,-1.));
#12672=DIRECTION('center_axis',(0.,0.,1.));
#12673=DIRECTION('ref_axis',(-1.,0.,0.));
#12674=DIRECTION('center_axis',(0.,0.,-1.));
#12675=DIRECTION('ref_axis',(-1.,0.,0.));
#12676=DIRECTION('center_axis',(0.,0.,-1.));
#12677=DIRECTION('ref_axis',(-1.,0.,0.));
#12678=DIRECTION('',(0.,0.,-1.));
#12679=DIRECTION('center_axis',(0.,0.,1.));
#12680=DIRECTION('ref_axis',(-1.,0.,0.));
#12681=DIRECTION('',(0.,0.,1.));
#12682=DIRECTION('center_axis',(0.,0.,1.));
#12683=DIRECTION('ref_axis',(-1.,0.,0.));
#12684=DIRECTION('',(0.,0.,-1.));
#12685=DIRECTION('center_axis',(0.,0.,1.));
#12686=DIRECTION('ref_axis',(-1.,0.,0.));
#12687=DIRECTION('center_axis',(0.,0.,-1.));
#12688=DIRECTION('ref_axis',(-2.22044604925031E-16,-1.,0.));
#12689=DIRECTION('',(1.,-2.22044604925031E-16,0.));
#12690=DIRECTION('',(-2.22044604925031E-16,-1.,0.));
#12691=DIRECTION('',(-1.,2.22044604925031E-16,0.));
#12692=DIRECTION('center_axis',(0.,0.,1.));
#12693=DIRECTION('ref_axis',(-1.,0.,0.));
#12694=DIRECTION('',(-1.,2.22044604925031E-16,0.));
#12695=DIRECTION('center_axis',(0.,0.,1.));
#12696=DIRECTION('ref_axis',(-1.,0.,0.));
#12697=DIRECTION('',(-1.,2.22044604925031E-16,0.));
#12698=DIRECTION('center_axis',(0.,0.,1.));
#12699=DIRECTION('ref_axis',(-1.,0.,0.));
#12700=DIRECTION('',(-1.,2.22044604925031E-16,0.));
#12701=DIRECTION('center_axis',(0.,0.,1.));
#12702=DIRECTION('ref_axis',(-1.,0.,0.));
#12703=DIRECTION('',(-1.,2.22044604925031E-16,0.));
#12704=DIRECTION('',(2.22044604925031E-16,1.,0.));
#12705=DIRECTION('',(1.,-2.22044604925031E-16,0.));
#12706=DIRECTION('center_axis',(0.,0.,1.));
#12707=DIRECTION('ref_axis',(-1.,0.,0.));
#12708=DIRECTION('',(1.,-2.22044604925031E-16,0.));
#12709=DIRECTION('center_axis',(0.,0.,1.));
#12710=DIRECTION('ref_axis',(-1.,0.,0.));
#12711=DIRECTION('center_axis',(0.,0.,1.));
#12712=DIRECTION('ref_axis',(-1.,0.,0.));
#12713=DIRECTION('',(1.,-2.22044604925031E-16,0.));
#12714=DIRECTION('center_axis',(0.,0.,1.));
#12715=DIRECTION('ref_axis',(-1.,0.,0.));
#12716=DIRECTION('center_axis',(0.,0.,1.));
#12717=DIRECTION('ref_axis',(-1.,0.,0.));
#12718=DIRECTION('',(1.,-2.22044604925031E-16,0.));
#12719=DIRECTION('center_axis',(0.,0.,1.));
#12720=DIRECTION('ref_axis',(-1.,0.,0.));
#12721=DIRECTION('center_axis',(0.,0.,1.));
#12722=DIRECTION('ref_axis',(-1.,0.,0.));
#12723=DIRECTION('',(1.,-2.22044604925031E-16,0.));
#12724=DIRECTION('center_axis',(-1.,2.22044604925031E-16,0.));
#12725=DIRECTION('ref_axis',(-1.57009245868376E-16,-0.707106781186541,-0.707106781186554));
#12726=DIRECTION('',(-1.,2.22044604925031E-16,0.));
#12727=DIRECTION('center_axis',(-1.,2.22044604925031E-16,0.));
#12728=DIRECTION('ref_axis',(-2.22044604925031E-16,-1.,0.));
#12729=DIRECTION('center_axis',(-2.22044604925031E-16,-1.,0.));
#12730=DIRECTION('ref_axis',(0.,0.,1.));
#12731=DIRECTION('',(1.,-2.22044604925031E-16,0.));
#12732=DIRECTION('',(0.,0.,1.));
#12733=DIRECTION('center_axis',(1.,-2.22044604925031E-16,0.));
#12734=DIRECTION('ref_axis',(1.57009245868376E-16,0.707106781186541,0.707106781186554));
#12735=DIRECTION('',(-1.,2.22044604925031E-16,0.));
#12736=DIRECTION('center_axis',(1.,-2.22044604925031E-16,0.));
#12737=DIRECTION('ref_axis',(0.,0.,1.));
#12738=DIRECTION('center_axis',(0.,0.,-1.));
#12739=DIRECTION('ref_axis',(-1.,0.,0.));
#12740=DIRECTION('center_axis',(0.,0.,-1.));
#12741=DIRECTION('ref_axis',(-1.,0.,0.));
#12742=DIRECTION('',(0.,0.,-1.));
#12743=DIRECTION('',(0.,0.,-1.));
#12744=DIRECTION('center_axis',(0.,0.,1.));
#12745=DIRECTION('ref_axis',(-1.,0.,0.));
#12746=DIRECTION('',(0.,0.,1.));
#12747=DIRECTION('center_axis',(0.,0.,-1.));
#12748=DIRECTION('ref_axis',(-1.,0.,0.));
#12749=DIRECTION('center_axis',(0.,0.,-1.));
#12750=DIRECTION('ref_axis',(-1.,0.,0.));
#12751=DIRECTION('',(0.,0.,-1.));
#12752=DIRECTION('center_axis',(0.,0.,1.));
#12753=DIRECTION('ref_axis',(-1.,0.,0.));
#12754=DIRECTION('center_axis',(0.,0.,-1.));
#12755=DIRECTION('ref_axis',(-1.,0.,0.));
#12756=DIRECTION('center_axis',(0.,0.,-1.));
#12757=DIRECTION('ref_axis',(-1.,0.,0.));
#12758=DIRECTION('',(0.,0.,-1.));
#12759=DIRECTION('center_axis',(0.,0.,1.));
#12760=DIRECTION('ref_axis',(-1.,0.,0.));
#12761=DIRECTION('center_axis',(0.,0.,-1.));
#12762=DIRECTION('ref_axis',(-1.,0.,0.));
#12763=DIRECTION('center_axis',(0.,0.,-1.));
#12764=DIRECTION('ref_axis',(-1.,0.,0.));
#12765=DIRECTION('',(0.,0.,-1.));
#12766=DIRECTION('center_axis',(0.,0.,1.));
#12767=DIRECTION('ref_axis',(-1.,0.,0.));
#12768=DIRECTION('',(0.,0.,-1.));
#12769=DIRECTION('',(0.,0.,1.));
#12770=DIRECTION('center_axis',(0.,0.,1.));
#12771=DIRECTION('ref_axis',(-1.,0.,0.));
#12772=DIRECTION('center_axis',(0.,0.,-1.));
#12773=DIRECTION('ref_axis',(-1.,0.,0.));
#12774=DIRECTION('center_axis',(0.,0.,-1.));
#12775=DIRECTION('ref_axis',(-1.,0.,0.));
#12776=DIRECTION('',(0.,0.,-1.));
#12777=DIRECTION('center_axis',(0.,0.,1.));
#12778=DIRECTION('ref_axis',(-1.,0.,0.));
#12779=DIRECTION('center_axis',(0.,0.,-1.));
#12780=DIRECTION('ref_axis',(-1.,0.,0.));
#12781=DIRECTION('center_axis',(0.,0.,-1.));
#12782=DIRECTION('ref_axis',(-1.,0.,0.));
#12783=DIRECTION('',(0.,0.,-1.));
#12784=DIRECTION('center_axis',(0.,0.,1.));
#12785=DIRECTION('ref_axis',(-1.,0.,0.));
#12786=DIRECTION('',(0.,0.,-1.));
#12787=DIRECTION('',(0.,0.,1.));
#12788=DIRECTION('center_axis',(0.,0.,1.));
#12789=DIRECTION('ref_axis',(-1.,0.,0.));
#12790=DIRECTION('center_axis',(0.,0.,-1.));
#12791=DIRECTION('ref_axis',(-1.,0.,0.));
#12792=DIRECTION('center_axis',(0.,0.,-1.));
#12793=DIRECTION('ref_axis',(-1.,0.,0.));
#12794=DIRECTION('',(0.,0.,-1.));
#12795=DIRECTION('center_axis',(0.,0.,1.));
#12796=DIRECTION('ref_axis',(-1.,0.,0.));
#12797=DIRECTION('center_axis',(0.,0.,-1.));
#12798=DIRECTION('ref_axis',(-1.,0.,0.));
#12799=DIRECTION('center_axis',(0.,0.,-1.));
#12800=DIRECTION('ref_axis',(-1.,0.,0.));
#12801=DIRECTION('',(0.,0.,-1.));
#12802=DIRECTION('center_axis',(0.,0.,1.));
#12803=DIRECTION('ref_axis',(-1.,0.,0.));
#12804=DIRECTION('',(0.,0.,-1.));
#12805=DIRECTION('',(0.,0.,1.));
#12806=DIRECTION('center_axis',(0.,0.,1.));
#12807=DIRECTION('ref_axis',(-1.,0.,0.));
#12808=DIRECTION('center_axis',(0.,0.,-1.));
#12809=DIRECTION('ref_axis',(-1.,0.,0.));
#12810=DIRECTION('center_axis',(0.,0.,-1.));
#12811=DIRECTION('ref_axis',(-1.,0.,0.));
#12812=DIRECTION('',(0.,0.,-1.));
#12813=DIRECTION('center_axis',(0.,0.,1.));
#12814=DIRECTION('ref_axis',(-1.,0.,0.));
#12815=DIRECTION('center_axis',(0.,0.,-1.));
#12816=DIRECTION('ref_axis',(-1.,0.,0.));
#12817=DIRECTION('center_axis',(0.,0.,-1.));
#12818=DIRECTION('ref_axis',(-1.,0.,0.));
#12819=DIRECTION('',(0.,0.,-1.));
#12820=DIRECTION('',(0.,0.,-1.));
#12821=DIRECTION('center_axis',(0.,0.,1.));
#12822=DIRECTION('ref_axis',(-1.,0.,0.));
#12823=DIRECTION('',(0.,0.,1.));
#12824=DIRECTION('center_axis',(0.,0.,-1.));
#12825=DIRECTION('ref_axis',(-1.,0.,0.));
#12826=DIRECTION('center_axis',(0.,0.,-1.));
#12827=DIRECTION('ref_axis',(-1.,0.,0.));
#12828=DIRECTION('',(0.,0.,-1.));
#12829=DIRECTION('center_axis',(0.,0.,1.));
#12830=DIRECTION('ref_axis',(-1.,0.,0.));
#12831=DIRECTION('center_axis',(0.,0.,-1.));
#12832=DIRECTION('ref_axis',(-1.,0.,0.));
#12833=DIRECTION('center_axis',(0.,0.,-1.));
#12834=DIRECTION('ref_axis',(-1.,0.,0.));
#12835=DIRECTION('',(0.,0.,-1.));
#12836=DIRECTION('center_axis',(0.,0.,1.));
#12837=DIRECTION('ref_axis',(-1.,0.,0.));
#12838=DIRECTION('',(0.,0.,-1.));
#12839=DIRECTION('',(0.,0.,1.));
#12840=DIRECTION('center_axis',(0.,0.,1.));
#12841=DIRECTION('ref_axis',(-1.,0.,0.));
#12842=DIRECTION('center_axis',(0.,0.,-1.));
#12843=DIRECTION('ref_axis',(-1.,0.,0.));
#12844=DIRECTION('center_axis',(0.,0.,-1.));
#12845=DIRECTION('ref_axis',(-1.,0.,0.));
#12846=DIRECTION('',(0.,0.,-1.));
#12847=DIRECTION('center_axis',(0.,0.,1.));
#12848=DIRECTION('ref_axis',(-1.,0.,0.));
#12849=DIRECTION('',(0.,0.,1.));
#12850=DIRECTION('center_axis',(0.,0.,1.));
#12851=DIRECTION('ref_axis',(-1.,0.,0.));
#12852=DIRECTION('',(0.,0.,-1.));
#12853=DIRECTION('center_axis',(0.,0.,1.));
#12854=DIRECTION('ref_axis',(-1.,0.,0.));
#12855=DIRECTION('center_axis',(-1.57009245868377E-16,-0.707106781186548,
-0.707106781186548));
#12856=DIRECTION('ref_axis',(0.,0.707106781186547,-0.707106781186547));
#12857=DIRECTION('center_axis',(0.,0.,1.));
#12858=DIRECTION('ref_axis',(-1.,0.,0.));
#12859=DIRECTION('center_axis',(-1.57009245868377E-16,-0.707106781186548,
-0.707106781186548));
#12860=DIRECTION('ref_axis',(0.,0.707106781186547,-0.707106781186547));
#12861=DIRECTION('center_axis',(0.,0.,1.));
#12862=DIRECTION('ref_axis',(-1.,0.,0.));
#12863=DIRECTION('center_axis',(0.,0.,-1.));
#12864=DIRECTION('ref_axis',(-1.,0.,0.));
#12865=DIRECTION('center_axis',(0.,0.,-1.));
#12866=DIRECTION('ref_axis',(-1.,0.,0.));
#12867=DIRECTION('',(0.,0.,-1.));
#12868=DIRECTION('center_axis',(0.,0.,1.));
#12869=DIRECTION('ref_axis',(-1.,0.,0.));
#12870=DIRECTION('',(0.,0.,1.));
#12871=DIRECTION('',(0.,0.,-1.));
#12872=DIRECTION('center_axis',(0.,0.,1.));
#12873=DIRECTION('ref_axis',(-1.,0.,0.));
#12874=DIRECTION('center_axis',(0.,0.,-1.));
#12875=DIRECTION('ref_axis',(-1.,0.,0.));
#12876=DIRECTION('center_axis',(0.,0.,-1.));
#12877=DIRECTION('ref_axis',(-1.,0.,0.));
#12878=DIRECTION('',(0.,0.,-1.));
#12879=DIRECTION('center_axis',(0.,0.,1.));
#12880=DIRECTION('ref_axis',(-1.,0.,0.));
#12881=DIRECTION('',(0.,0.,1.));
#12882=DIRECTION('center_axis',(0.,0.,1.));
#12883=DIRECTION('ref_axis',(-1.,0.,0.));
#12884=DIRECTION('',(0.,0.,-1.));
#12885=DIRECTION('center_axis',(0.,0.,1.));
#12886=DIRECTION('ref_axis',(-1.,0.,0.));
#12887=DIRECTION('center_axis',(-1.57009245868377E-16,-0.707106781186548,
-0.707106781186548));
#12888=DIRECTION('ref_axis',(0.,0.707106781186547,-0.707106781186547));
#12889=DIRECTION('center_axis',(0.,0.,1.));
#12890=DIRECTION('ref_axis',(-1.,0.,0.));
#12891=DIRECTION('center_axis',(-1.57009245868377E-16,-0.707106781186548,
-0.707106781186548));
#12892=DIRECTION('ref_axis',(0.,0.707106781186547,-0.707106781186547));
#12893=DIRECTION('center_axis',(0.,0.,1.));
#12894=DIRECTION('ref_axis',(-1.,0.,0.));
#12895=DIRECTION('center_axis',(0.,0.,-1.));
#12896=DIRECTION('ref_axis',(-1.,0.,0.));
#12897=DIRECTION('center_axis',(0.,0.,-1.));
#12898=DIRECTION('ref_axis',(-1.,0.,0.));
#12899=DIRECTION('',(0.,0.,-1.));
#12900=DIRECTION('center_axis',(0.,0.,1.));
#12901=DIRECTION('ref_axis',(-1.,0.,0.));
#12902=DIRECTION('',(0.,0.,1.));
#12903=DIRECTION('center_axis',(0.,0.,1.));
#12904=DIRECTION('ref_axis',(-1.,0.,0.));
#12905=DIRECTION('',(0.,0.,-1.));
#12906=DIRECTION('center_axis',(0.,0.,1.));
#12907=DIRECTION('ref_axis',(-1.,0.,0.));
#12908=DIRECTION('center_axis',(-1.57009245868377E-16,-0.707106781186548,
-0.707106781186548));
#12909=DIRECTION('ref_axis',(0.,0.707106781186547,-0.707106781186547));
#12910=DIRECTION('center_axis',(0.,0.,1.));
#12911=DIRECTION('ref_axis',(-1.,0.,0.));
#12912=DIRECTION('center_axis',(-1.57009245868377E-16,-0.707106781186548,
-0.707106781186548));
#12913=DIRECTION('ref_axis',(0.,0.707106781186547,-0.707106781186547));
#12914=DIRECTION('center_axis',(0.,0.,1.));
#12915=DIRECTION('ref_axis',(-1.,0.,0.));
#12916=DIRECTION('center_axis',(0.,0.,-1.));
#12917=DIRECTION('ref_axis',(-1.,0.,0.));
#12918=DIRECTION('center_axis',(0.,0.,-1.));
#12919=DIRECTION('ref_axis',(-1.,0.,0.));
#12920=DIRECTION('',(0.,0.,-1.));
#12921=DIRECTION('center_axis',(0.,0.,1.));
#12922=DIRECTION('ref_axis',(-1.,0.,0.));
#12923=DIRECTION('',(0.,0.,1.));
#12924=DIRECTION('center_axis',(0.,0.,1.));
#12925=DIRECTION('ref_axis',(-1.,0.,0.));
#12926=DIRECTION('',(0.,0.,-1.));
#12927=DIRECTION('center_axis',(0.,0.,1.));
#12928=DIRECTION('ref_axis',(-1.,0.,0.));
#12929=DIRECTION('center_axis',(-1.57009245868377E-16,-0.707106781186548,
-0.707106781186548));
#12930=DIRECTION('ref_axis',(0.,0.707106781186547,-0.707106781186547));
#12931=DIRECTION('center_axis',(0.,0.,1.));
#12932=DIRECTION('ref_axis',(-1.,0.,0.));
#12933=DIRECTION('center_axis',(-1.57009245868377E-16,-0.707106781186548,
-0.707106781186548));
#12934=DIRECTION('ref_axis',(0.,0.707106781186547,-0.707106781186547));
#12935=DIRECTION('center_axis',(0.,0.,1.));
#12936=DIRECTION('ref_axis',(-1.,0.,0.));
#12937=DIRECTION('center_axis',(0.,0.,-1.));
#12938=DIRECTION('ref_axis',(-1.,0.,0.));
#12939=DIRECTION('center_axis',(0.,0.,-1.));
#12940=DIRECTION('ref_axis',(-1.,0.,0.));
#12941=DIRECTION('',(0.,0.,-1.));
#12942=DIRECTION('center_axis',(0.,0.,1.));
#12943=DIRECTION('ref_axis',(-1.,0.,0.));
#12944=DIRECTION('center_axis',(0.,0.,-1.));
#12945=DIRECTION('ref_axis',(-1.,0.,0.));
#12946=DIRECTION('center_axis',(0.,0.,-1.));
#12947=DIRECTION('ref_axis',(-1.,0.,0.));
#12948=DIRECTION('',(0.,0.,-1.));
#12949=DIRECTION('',(0.,0.,-1.));
#12950=DIRECTION('center_axis',(0.,0.,1.));
#12951=DIRECTION('ref_axis',(-1.,0.,0.));
#12952=DIRECTION('',(0.,0.,1.));
#12953=DIRECTION('center_axis',(-1.,2.22044604925031E-16,0.));
#12954=DIRECTION('ref_axis',(1.57009245868377E-16,0.707106781186544,0.707106781186551));
#12955=DIRECTION('',(1.,-2.22044604925031E-16,0.));
#12956=DIRECTION('center_axis',(-1.,2.22044604925031E-16,0.));
#12957=DIRECTION('ref_axis',(1.57009245868377E-16,0.707106781186544,0.707106781186551));
#12958=DIRECTION('center_axis',(1.,-2.22044604925031E-16,0.));
#12959=DIRECTION('ref_axis',(0.,0.,1.));
#12960=DIRECTION('',(1.,-2.22044604925031E-16,0.));
#12961=DIRECTION('center_axis',(-1.,2.22044604925031E-16,0.));
#12962=DIRECTION('ref_axis',(1.57009245868377E-16,0.707106781186544,0.707106781186551));
#12963=DIRECTION('',(1.,-2.22044604925031E-16,0.));
#12964=DIRECTION('center_axis',(-1.,2.22044604925031E-16,0.));
#12965=DIRECTION('ref_axis',(1.57009245868377E-16,0.707106781186544,0.707106781186551));
#12966=DIRECTION('',(1.,-2.22044604925031E-16,0.));
#12967=DIRECTION('center_axis',(-1.,2.22044604925031E-16,0.));
#12968=DIRECTION('ref_axis',(2.22044604925031E-16,1.,0.));
#12969=DIRECTION('center_axis',(-1.,2.22044604925031E-16,0.));
#12970=DIRECTION('ref_axis',(1.57009245868377E-16,0.707106781186544,0.707106781186551));
#12971=DIRECTION('',(1.,-2.22044604925031E-16,0.));
#12972=DIRECTION('center_axis',(-2.22044604925031E-16,-1.,0.));
#12973=DIRECTION('ref_axis',(0.,0.,1.));
#12974=DIRECTION('',(-1.,2.22044604925031E-16,0.));
#12975=DIRECTION('',(0.,0.,-1.));
#12976=DIRECTION('center_axis',(-2.22044604925031E-16,-1.,0.));
#12977=DIRECTION('ref_axis',(0.,0.,1.));
#12978=DIRECTION('',(-1.,2.22044604925031E-16,0.));
#12979=DIRECTION('center_axis',(-2.22044604925031E-16,-1.,0.));
#12980=DIRECTION('ref_axis',(0.,0.,1.));
#12981=DIRECTION('',(0.,0.,1.));
#12982=DIRECTION('',(-1.,2.22044604925031E-16,0.));
#12983=DIRECTION('center_axis',(-2.22044604925031E-16,-1.,0.));
#12984=DIRECTION('ref_axis',(0.,0.,1.));
#12985=DIRECTION('',(-1.,2.22044604925031E-16,0.));
#12986=DIRECTION('center_axis',(-1.,2.22044604925031E-16,0.));
#12987=DIRECTION('ref_axis',(-1.57009245868377E-16,-0.707106781186546,-0.707106781186549));
#12988=DIRECTION('',(1.,-2.22044604925031E-16,0.));
#12989=DIRECTION('center_axis',(-1.,2.22044604925031E-16,0.));
#12990=DIRECTION('ref_axis',(-1.57009245868377E-16,-0.707106781186546,-0.707106781186549));
#12991=DIRECTION('center_axis',(-1.,2.22044604925031E-16,0.));
#12992=DIRECTION('ref_axis',(-2.22044604925031E-16,-1.,0.));
#12993=DIRECTION('',(1.,-2.22044604925031E-16,0.));
#12994=DIRECTION('center_axis',(-1.,2.22044604925031E-16,0.));
#12995=DIRECTION('ref_axis',(-1.57009245868377E-16,-0.707106781186546,-0.707106781186549));
#12996=DIRECTION('',(1.,-2.22044604925031E-16,0.));
#12997=DIRECTION('center_axis',(-1.,2.22044604925031E-16,0.));
#12998=DIRECTION('ref_axis',(-1.57009245868377E-16,-0.707106781186546,-0.707106781186549));
#12999=DIRECTION('',(1.,-2.22044604925031E-16,0.));
#13000=DIRECTION('center_axis',(1.,-2.22044604925031E-16,0.));
#13001=DIRECTION('ref_axis',(0.,0.,-1.));
#13002=DIRECTION('center_axis',(-1.,2.22044604925031E-16,0.));
#13003=DIRECTION('ref_axis',(1.57009245868377E-16,0.707106781186547,-0.707106781186548));
#13004=DIRECTION('',(-1.,2.22044604925031E-16,0.));
#13005=DIRECTION('center_axis',(-1.,2.22044604925031E-16,0.));
#13006=DIRECTION('ref_axis',(0.,0.,-1.));
#13007=DIRECTION('',(1.,-2.22044604925031E-16,0.));
#13008=DIRECTION('center_axis',(-1.,2.22044604925031E-16,0.));
#13009=DIRECTION('ref_axis',(1.57009245868377E-16,0.707106781186547,-0.707106781186548));
#13010=DIRECTION('',(-1.,2.22044604925031E-16,0.));
#13011=DIRECTION('',(1.,-2.22044604925031E-16,0.));
#13012=DIRECTION('center_axis',(-1.,2.22044604925031E-16,0.));
#13013=DIRECTION('ref_axis',(1.57009245868377E-16,0.707106781186547,-0.707106781186548));
#13014=DIRECTION('',(1.,-2.22044604925031E-16,0.));
#13015=DIRECTION('center_axis',(1.,-2.22044604925031E-16,0.));
#13016=DIRECTION('ref_axis',(2.22044604925031E-16,1.,0.));
#13017=DIRECTION('',(-1.,2.22044604925031E-16,0.));
#13018=DIRECTION('center_axis',(-1.,2.22044604925031E-16,0.));
#13019=DIRECTION('ref_axis',(1.57009245868377E-16,0.707106781186547,-0.707106781186548));
#13020=DIRECTION('',(1.,-2.22044604925031E-16,0.));
#13021=DIRECTION('',(-1.,2.22044604925031E-16,0.));
#13022=DIRECTION('center_axis',(-1.,2.22044604925031E-16,0.));
#13023=DIRECTION('ref_axis',(1.57009245868377E-16,0.707106781186547,-0.707106781186548));
#13024=DIRECTION('',(-1.,2.22044604925031E-16,0.));
#13025=DIRECTION('',(1.,-2.22044604925031E-16,0.));
#13026=DIRECTION('center_axis',(2.22044604925031E-16,1.,0.));
#13027=DIRECTION('ref_axis',(0.,0.,-1.));
#13028=DIRECTION('',(0.,0.,-1.));
#13029=DIRECTION('',(-1.,2.22044604925031E-16,0.));
#13030=DIRECTION('center_axis',(2.22044604925031E-16,1.,0.));
#13031=DIRECTION('ref_axis',(0.,0.,-1.));
#13032=DIRECTION('',(-1.,2.22044604925031E-16,0.));
#13033=DIRECTION('center_axis',(2.22044604925031E-16,1.,0.));
#13034=DIRECTION('ref_axis',(0.,0.,-1.));
#13035=DIRECTION('',(-1.,2.22044604925031E-16,0.));
#13036=DIRECTION('',(0.,0.,1.));
#13037=DIRECTION('center_axis',(2.22044604925031E-16,1.,0.));
#13038=DIRECTION('ref_axis',(0.,0.,-1.));
#13039=DIRECTION('',(-1.,2.22044604925031E-16,0.));
#13040=DIRECTION('center_axis',(2.22044604925031E-16,1.,0.));
#13041=DIRECTION('ref_axis',(0.,0.,-1.));
#13042=DIRECTION('',(-1.,2.22044604925031E-16,0.));
#13043=DIRECTION('center_axis',(-1.,2.22044604925031E-16,0.));
#13044=DIRECTION('ref_axis',(-2.05142465794791E-16,-0.923879532511288,0.382683432365088));
#13045=DIRECTION('',(-1.,2.22044604925031E-16,0.));
#13046=DIRECTION('center_axis',(1.,-2.22044604925031E-16,0.));
#13047=DIRECTION('ref_axis',(-1.57009245868377E-16,-0.707106781186548,-0.707106781186548));
#13048=DIRECTION('',(1.,-2.22044604925031E-16,0.));
#13049=DIRECTION('center_axis',(-1.,2.22044604925031E-16,0.));
#13050=DIRECTION('ref_axis',(-2.05142465794791E-16,-0.923879532511288,0.382683432365088));
#13051=DIRECTION('',(-1.,2.22044604925031E-16,0.));
#13052=DIRECTION('',(1.,-2.22044604925031E-16,0.));
#13053=DIRECTION('center_axis',(-1.,2.22044604925031E-16,0.));
#13054=DIRECTION('ref_axis',(-2.05142465794791E-16,-0.923879532511288,0.382683432365088));
#13055=DIRECTION('',(1.,-2.22044604925031E-16,0.));
#13056=DIRECTION('center_axis',(-1.,5.04650032828059E-14,0.));
#13057=DIRECTION('ref_axis',(0.,0.,1.));
#13058=DIRECTION('',(-1.,2.22044604925031E-16,0.));
#13059=DIRECTION('center_axis',(-1.,2.22044604925031E-16,0.));
#13060=DIRECTION('ref_axis',(-2.05142465794791E-16,-0.923879532511288,0.382683432365088));
#13061=DIRECTION('',(1.,-2.22044604925031E-16,0.));
#13062=DIRECTION('',(-1.,2.22044604925031E-16,0.));
#13063=DIRECTION('center_axis',(-1.,2.22044604925031E-16,0.));
#13064=DIRECTION('ref_axis',(-1.57009245868377E-16,-0.707106781186548,0.707106781186548));
#13065=DIRECTION('center_axis',(1.,-2.22044604925031E-16,0.));
#13066=DIRECTION('ref_axis',(-2.22044604925031E-16,-1.,0.));
#13067=DIRECTION('',(1.,-2.22044604925031E-16,0.));
#13068=DIRECTION('center_axis',(-1.,2.22044604925031E-16,0.));
#13069=DIRECTION('ref_axis',(-1.57009245868377E-16,-0.707106781186548,0.707106781186548));
#13070=DIRECTION('',(1.,-2.22044604925031E-16,0.));
#13071=DIRECTION('center_axis',(-1.,2.22044604925031E-16,0.));
#13072=DIRECTION('ref_axis',(-1.57009245868377E-16,-0.707106781186548,0.707106781186548));
#13073=DIRECTION('',(1.,-2.22044604925031E-16,0.));
#13074=DIRECTION('center_axis',(-1.,2.22044604925031E-16,0.));
#13075=DIRECTION('ref_axis',(0.,0.,1.));
#13076=DIRECTION('center_axis',(-1.,2.22044604925031E-16,0.));
#13077=DIRECTION('ref_axis',(-1.57009245868377E-16,-0.707106781186548,0.707106781186548));
#13078=DIRECTION('',(1.,-2.22044604925031E-16,0.));
#13079=DIRECTION('center_axis',(-1.,2.22044604925031E-16,0.));
#13080=DIRECTION('ref_axis',(-1.57009245868377E-16,-0.707106781186548,0.707106781186548));
#13081=DIRECTION('',(1.,-2.22044604925031E-16,0.));
#13082=DIRECTION('center_axis',(1.57009245868377E-16,0.707106781186548,
0.707106781186548));
#13083=DIRECTION('ref_axis',(1.57009245868377E-16,0.707106781186548,-0.707106781186548));
#13084=DIRECTION('',(1.,-2.22044604925031E-16,0.));
#13085=DIRECTION('',(1.57009245868377E-16,0.707106781186548,-0.707106781186548));
#13086=DIRECTION('center_axis',(1.57009245868377E-16,0.707106781186548,
0.707106781186548));
#13087=DIRECTION('ref_axis',(1.57009245868377E-16,0.707106781186548,-0.707106781186548));
#13088=DIRECTION('',(1.,-2.22044604925031E-16,0.));
#13089=DIRECTION('center_axis',(1.57009245868377E-16,0.707106781186548,
0.707106781186548));
#13090=DIRECTION('ref_axis',(1.57009245868377E-16,0.707106781186548,-0.707106781186548));
#13091=DIRECTION('',(-1.57009245868377E-16,-0.707106781186548,0.707106781186548));
#13092=DIRECTION('',(1.,-2.22044604925031E-16,0.));
#13093=DIRECTION('center_axis',(1.57009245868377E-16,0.707106781186548,
0.707106781186548));
#13094=DIRECTION('ref_axis',(1.57009245868377E-16,0.707106781186548,-0.707106781186548));
#13095=DIRECTION('',(1.,-2.22044604925031E-16,0.));
#13096=DIRECTION('center_axis',(0.,0.,-1.));
#13097=DIRECTION('ref_axis',(-2.22044604925031E-16,-1.,0.));
#13098=DIRECTION('',(-1.,2.22044604925031E-16,0.));
#13099=DIRECTION('',(2.22044604925031E-16,1.,0.));
#13100=DIRECTION('center_axis',(0.,0.,-1.));
#13101=DIRECTION('ref_axis',(-2.22044604925031E-16,-1.,0.));
#13102=DIRECTION('',(-2.22044604925031E-16,-1.,0.));
#13103=DIRECTION('',(-1.,2.22044604925031E-16,0.));
#13104=DIRECTION('center_axis',(0.,0.,-1.));
#13105=DIRECTION('ref_axis',(-2.22044604925031E-16,-1.,0.));
#13106=DIRECTION('',(-1.,2.22044604925031E-16,0.));
#13107=DIRECTION('center_axis',(0.,0.,-1.));
#13108=DIRECTION('ref_axis',(-2.22044604925031E-16,-1.,0.));
#13109=DIRECTION('',(-1.,2.22044604925031E-16,0.));
#13110=DIRECTION('center_axis',(-1.,2.22044604925031E-16,0.));
#13111=DIRECTION('ref_axis',(2.05142465794791E-16,0.923879532511283,-0.382683432365098));
#13112=DIRECTION('center_axis',(-1.,2.22044604925031E-16,0.));
#13113=DIRECTION('ref_axis',(0.,0.,-1.));
#13114=DIRECTION('center_axis',(-1.,2.22044604925031E-16,0.));
#13115=DIRECTION('ref_axis',(2.05142465794791E-16,0.923879532511283,-0.382683432365098));
#13116=DIRECTION('center_axis',(-1.,2.22044604925031E-16,0.));
#13117=DIRECTION('ref_axis',(2.05142465794791E-16,0.923879532511283,-0.382683432365098));
#13118=DIRECTION('center_axis',(1.,-7.1276318180935E-14,7.105427357601E-14));
#13119=DIRECTION('ref_axis',(1.57009245868377E-16,0.707106781186548,0.707106781186548));
#13120=DIRECTION('center_axis',(-1.,2.22044604925031E-16,0.));
#13121=DIRECTION('ref_axis',(2.05142465794791E-16,0.923879532511283,-0.382683432365098));
#13122=DIRECTION('center_axis',(0.,0.,1.));
#13123=DIRECTION('ref_axis',(2.22044604925031E-16,1.,0.));
#13124=DIRECTION('',(-1.,2.22044604925031E-16,0.));
#13125=DIRECTION('',(-1.,2.22044604925031E-16,0.));
#13126=DIRECTION('',(-1.,2.22044604925031E-16,0.));
#13127=DIRECTION('',(-1.,2.22044604925031E-16,0.));
#13128=DIRECTION('',(-1.,2.22044604925031E-16,0.));
#13129=DIRECTION('',(2.22044604925031E-16,1.,0.));
#13130=DIRECTION('',(1.,-2.22044604925031E-16,0.));
#13131=DIRECTION('',(-2.22044604925031E-16,-1.,0.));
#13132=DIRECTION('center_axis',(1.,-2.22044604925031E-16,0.));
#13133=DIRECTION('ref_axis',(1.57009245868376E-16,0.707106781186541,0.707106781186554));
#13134=DIRECTION('',(1.,-2.22044604925031E-16,0.));
#13135=DIRECTION('center_axis',(1.,-2.22044604925031E-16,0.));
#13136=DIRECTION('ref_axis',(1.57009245868376E-16,0.707106781186541,0.707106781186554));
#13137=DIRECTION('',(1.,-2.22044604925031E-16,0.));
#13138=DIRECTION('center_axis',(-1.,2.22044604925031E-16,0.));
#13139=DIRECTION('ref_axis',(2.22044604925031E-16,1.,0.));
#13140=DIRECTION('center_axis',(1.,-2.22044604925031E-16,0.));
#13141=DIRECTION('ref_axis',(1.57009245868376E-16,0.707106781186541,0.707106781186554));
#13142=DIRECTION('',(1.,-2.22044604925031E-16,0.));
#13143=DIRECTION('center_axis',(1.,-2.22044604925031E-16,0.));
#13144=DIRECTION('ref_axis',(1.57009245868376E-16,0.707106781186541,0.707106781186554));
#13145=DIRECTION('',(1.,-2.22044604925031E-16,0.));
#13146=DIRECTION('center_axis',(1.,-2.22044604925031E-16,0.));
#13147=DIRECTION('ref_axis',(1.57009245868376E-16,0.707106781186541,0.707106781186554));
#13148=DIRECTION('',(1.,-2.22044604925031E-16,0.));
#13149=DIRECTION('center_axis',(-2.22044604925031E-16,-1.,0.));
#13150=DIRECTION('ref_axis',(0.,0.,1.));
#13151=DIRECTION('',(-1.,2.22044604925031E-16,0.));
#13152=DIRECTION('',(0.,0.,-1.));
#13153=DIRECTION('center_axis',(-2.22044604925031E-16,-1.,0.));
#13154=DIRECTION('ref_axis',(0.,0.,1.));
#13155=DIRECTION('',(-1.,2.22044604925031E-16,0.));
#13156=DIRECTION('center_axis',(-2.22044604925031E-16,-1.,0.));
#13157=DIRECTION('ref_axis',(0.,0.,1.));
#13158=DIRECTION('',(-1.,2.22044604925031E-16,0.));
#13159=DIRECTION('center_axis',(-2.22044604925031E-16,-1.,0.));
#13160=DIRECTION('ref_axis',(0.,0.,1.));
#13161=DIRECTION('',(-1.,2.22044604925031E-16,0.));
#13162=DIRECTION('center_axis',(-1.,2.22044604925031E-16,0.));
#13163=DIRECTION('ref_axis',(-1.57009245868376E-16,-0.707106781186541,-0.707106781186554));
#13164=DIRECTION('center_axis',(-1.,2.22044604925031E-16,0.));
#13165=DIRECTION('ref_axis',(-1.57009245868376E-16,-0.707106781186541,-0.707106781186554));
#13166=DIRECTION('center_axis',(1.,-2.22044604925031E-16,0.));
#13167=DIRECTION('ref_axis',(0.,0.,-1.));
#13168=DIRECTION('center_axis',(-1.,2.22044604925031E-16,0.));
#13169=DIRECTION('ref_axis',(-1.57009245868376E-16,-0.707106781186541,-0.707106781186554));
#13170=DIRECTION('center_axis',(-1.,2.22044604925031E-16,0.));
#13171=DIRECTION('ref_axis',(-1.57009245868376E-16,-0.707106781186541,-0.707106781186554));
#13172=DIRECTION('center_axis',(0.,0.,-1.));
#13173=DIRECTION('ref_axis',(-2.22044604925031E-16,-1.,0.));
#13174=DIRECTION('',(1.,-2.22044604925031E-16,0.));
#13175=DIRECTION('',(-2.22044604925031E-16,-1.,0.));
#13176=DIRECTION('',(2.22044604925031E-16,1.,0.));
#13177=DIRECTION('center_axis',(0.,0.,1.));
#13178=DIRECTION('ref_axis',(2.22044604925031E-16,1.,0.));
#13179=DIRECTION('',(1.,-2.22044604925031E-16,0.));
#13180=DIRECTION('',(-2.22044604925031E-16,-1.,0.));
#13181=DIRECTION('',(-1.,2.22044604925031E-16,0.));
#13182=DIRECTION('',(2.22044604925031E-16,1.,0.));
#13183=DIRECTION('center_axis',(-0.538877990790891,0.827465426020391,0.15783370927044));
#13184=DIRECTION('ref_axis',(0.79410448776086,0.561516668266297,-0.232587819494442));
#13185=DIRECTION('center_axis',(1.57009245868378E-16,0.707106781186552,
-0.707106781186543));
#13186=DIRECTION('ref_axis',(1.,-2.22044604925031E-16,0.));
#13187=DIRECTION('center_axis',(2.22044604925031E-16,1.,0.));
#13188=DIRECTION('ref_axis',(0.,0.,-1.));
#13189=DIRECTION('center_axis',(0.53887799079092,0.827465426020364,0.157833709270477));
#13190=DIRECTION('ref_axis',(-0.794104487760813,0.561516668266353,-0.232587819494468));
#13191=DIRECTION('center_axis',(2.22044604925031E-16,1.,0.));
#13192=DIRECTION('ref_axis',(-1.,2.22044604925031E-16,0.));
#13193=DIRECTION('center_axis',(1.57009245868377E-16,0.707106781186548,
-0.707106781186548));
#13194=DIRECTION('ref_axis',(1.57009245868378E-16,0.707106781186548,0.707106781186548));
#13195=DIRECTION('center_axis',(-1.,2.22044604925031E-16,0.));
#13196=DIRECTION('ref_axis',(0.,0.,-1.));
#13197=DIRECTION('center_axis',(2.22044604925031E-16,1.,0.));
#13198=DIRECTION('ref_axis',(1.,-2.22044604925031E-16,0.));
#13199=DIRECTION('center_axis',(1.,-2.22044604925031E-16,0.));
#13200=DIRECTION('ref_axis',(-1.57009245868378E-16,-0.707106781186549,0.707106781186546));
#13201=DIRECTION('center_axis',(0.,0.,-1.));
#13202=DIRECTION('ref_axis',(2.22044604925031E-16,1.,0.));
#13203=DIRECTION('center_axis',(-2.22044604925031E-16,-1.,0.));
#13204=DIRECTION('ref_axis',(0.707106781186554,-1.57009245868379E-16,-0.707106781186541));
#13205=DIRECTION('',(-2.22044604925031E-16,-1.,0.));
#13206=DIRECTION('center_axis',(-1.,2.22044604925031E-16,3.5527136788003E-14));
#13207=DIRECTION('ref_axis',(-2.84217094304039E-14,0.,-1.));
#13208=DIRECTION('center_axis',(1.,-2.22044604925031E-16,0.));
#13209=DIRECTION('ref_axis',(-2.05142465794791E-16,-0.923879532511286,0.382683432365093));
#13210=DIRECTION('center_axis',(-2.49644700930708E-14,0.707106781186543,
-0.707106781186552));
#13211=DIRECTION('ref_axis',(1.57009245868378E-16,0.707106781186552,0.707106781186543));
#13212=DIRECTION('center_axis',(2.22044604925031E-16,1.,0.));
#13213=DIRECTION('ref_axis',(1.,-2.22044604925031E-16,0.));
#13214=DIRECTION('center_axis',(1.,-2.22044604925031E-16,0.));
#13215=DIRECTION('ref_axis',(0.,0.,1.));
#13216=DIRECTION('center_axis',(0.,0.,-1.));
#13217=DIRECTION('ref_axis',(-1.,2.22044604925031E-16,0.));
#13218=DIRECTION('center_axis',(-1.,2.22044604925031E-16,0.));
#13219=DIRECTION('ref_axis',(-1.57009245868378E-16,-0.707106781186549,0.707106781186546));
#13220=DIRECTION('center_axis',(2.22044604925031E-16,1.,0.));
#13221=DIRECTION('ref_axis',(0.,0.,-1.));
#13222=DIRECTION('center_axis',(1.,-2.22044604925031E-16,0.));
#13223=DIRECTION('ref_axis',(0.,0.,1.));
#13224=DIRECTION('center_axis',(-1.,2.22044604925031E-16,0.));
#13225=DIRECTION('ref_axis',(-2.05142465794794E-16,-0.9238795325113,0.382683432365059));
#13226=DIRECTION('center_axis',(2.22044604925031E-16,1.,0.));
#13227=DIRECTION('ref_axis',(0.,0.,-1.));
#13228=DIRECTION('center_axis',(1.57009245868376E-16,0.707106781186539,
-0.707106781186556));
#13229=DIRECTION('ref_axis',(-1.,2.22044604925031E-16,0.));
#13230=DIRECTION('center_axis',(-1.57009245868377E-16,-0.707106781186548,
0.707106781186548));
#13231=DIRECTION('ref_axis',(-0.707106781186551,0.499999999999995,0.500000000000001));
#13232=DIRECTION('',(-1.57009245868377E-16,-0.707106781186548,0.707106781186548));
#13233=DIRECTION('center_axis',(-0.408248290463856,0.816496580927733,0.408248290463856));
#13234=DIRECTION('ref_axis',(0.577350269189638,0.577350269189616,-0.577350269189623));
#13235=DIRECTION('center_axis',(0.,0.,-1.));
#13236=DIRECTION('ref_axis',(1.,-2.22044604925031E-16,0.));
#13237=DIRECTION('center_axis',(2.22044604925031E-16,1.,0.));
#13238=DIRECTION('ref_axis',(0.,0.,-1.));
#13239=DIRECTION('center_axis',(0.,0.,-1.));
#13240=DIRECTION('ref_axis',(0.707106781186554,0.707106781186541,0.));
#13241=DIRECTION('',(0.,0.,-1.));
#13242=DIRECTION('center_axis',(-0.408248290463858,-0.408248290463858,-0.816496580927731));
#13243=DIRECTION('ref_axis',(0.577350269189631,0.577350269189631,-0.577350269189616));
#13244=DIRECTION('center_axis',(0.,0.,-1.));
#13245=DIRECTION('ref_axis',(1.,-2.22044604925031E-16,0.));
#13246=DIRECTION('center_axis',(2.22044604925031E-16,1.,0.));
#13247=DIRECTION('ref_axis',(0.,0.,-1.));
#13248=DIRECTION('center_axis',(1.,-2.22044604925031E-16,0.));
#13249=DIRECTION('ref_axis',(2.22044604925031E-16,1.,0.));
#13250=DIRECTION('center_axis',(2.22044604925031E-16,1.,0.));
#13251=DIRECTION('ref_axis',(0.707106781186554,-1.57009245868379E-16,-0.707106781186541));
#13252=DIRECTION('',(-2.22044604925031E-16,-1.,0.));
#13253=DIRECTION('center_axis',(0.408248290463856,0.816496580927733,0.408248290463856));
#13254=DIRECTION('ref_axis',(-0.577350269189638,0.577350269189616,-0.577350269189623));
#13255=DIRECTION('center_axis',(2.22044604925031E-16,1.,0.));
#13256=DIRECTION('ref_axis',(-1.,2.22044604925031E-16,0.));
#13257=DIRECTION('center_axis',(0.,0.,-1.));
#13258=DIRECTION('ref_axis',(2.22044604925031E-16,1.,0.));
#13259=DIRECTION('center_axis',(0.408248290463854,-0.408248290463854,-0.816496580927736));
#13260=DIRECTION('ref_axis',(-0.577350269189616,0.577350269189645,-0.577350269189616));
#13261=DIRECTION('center_axis',(-1.,2.22044604925031E-16,0.));
#13262=DIRECTION('ref_axis',(0.,0.,-1.));
#13263=DIRECTION('center_axis',(2.22044604925031E-16,1.,1.77635683940026E-14));
#13264=DIRECTION('ref_axis',(-1.,2.22044604925031E-16,0.));
#13265=DIRECTION('center_axis',(0.,0.,-1.));
#13266=DIRECTION('ref_axis',(2.22044604925031E-16,1.,0.));
#13267=DIRECTION('center_axis',(-2.22044604925031E-16,-1.,0.));
#13268=DIRECTION('ref_axis',(-0.707106781186554,1.57009245868379E-16,-0.707106781186541));
#13269=DIRECTION('',(2.22044604925031E-16,1.,0.));
#13270=DIRECTION('center_axis',(0.408248290463856,0.816496580927733,-0.408248290463856));
#13271=DIRECTION('ref_axis',(0.577350269189638,-0.577350269189616,-0.577350269189623));
#13272=DIRECTION('center_axis',(-2.22044604925031E-16,-1.,0.));
#13273=DIRECTION('ref_axis',(1.,-2.22044604925031E-16,0.));
#13274=DIRECTION('center_axis',(-2.22044604925028E-15,4.93038065763125E-31,
-1.));
#13275=DIRECTION('ref_axis',(-2.22044604925031E-16,-1.,0.));
#13276=DIRECTION('center_axis',(-2.22044604925031E-16,-1.,0.));
#13277=DIRECTION('ref_axis',(0.707106781186553,-1.57009245868379E-16,-0.707106781186542));
#13278=DIRECTION('',(-2.22044604925031E-16,-1.,0.));
#13279=DIRECTION('center_axis',(-0.408248290463875,0.816496580927721,-0.408248290463861));
#13280=DIRECTION('ref_axis',(0.577350269189635,0.577350269189635,0.577350269189607));
#13281=DIRECTION('center_axis',(2.22044604925031E-16,1.,0.));
#13282=DIRECTION('ref_axis',(1.,-2.22044604925031E-16,0.));
#13283=DIRECTION('center_axis',(0.,0.,1.));
#13284=DIRECTION('ref_axis',(2.22044604925031E-16,1.,0.));
#13285=DIRECTION('center_axis',(1.,-2.22044604925031E-16,0.));
#13286=DIRECTION('ref_axis',(0.,0.,1.));
#13287=DIRECTION('center_axis',(0.,0.,1.));
#13288=DIRECTION('ref_axis',(0.707106781186548,0.707106781186547,0.));
#13289=DIRECTION('',(0.,0.,-1.));
#13290=DIRECTION('',(0.,0.,1.));
#13291=DIRECTION('center_axis',(-0.408248290463856,0.816496580927733,-0.408248290463856));
#13292=DIRECTION('ref_axis',(-0.577350269189638,-0.577350269189616,-0.577350269189623));
#13293=DIRECTION('center_axis',(-4.93038065763134E-31,-2.22044604925032E-15,
-1.));
#13294=DIRECTION('ref_axis',(-1.,2.22044604925031E-16,0.));
#13295=DIRECTION('center_axis',(-2.22044604925031E-16,-1.,0.));
#13296=DIRECTION('ref_axis',(0.,0.,-1.));
#13297=DIRECTION('center_axis',(-0.408248290463854,0.408248290463854,-0.816496580927736));
#13298=DIRECTION('ref_axis',(-0.577350269189616,0.577350269189645,0.577350269189616));
#13299=DIRECTION('center_axis',(-1.,2.22044604925031E-16,0.));
#13300=DIRECTION('ref_axis',(2.22044604925031E-16,1.,0.));
#13301=DIRECTION('center_axis',(0.,0.,1.));
#13302=DIRECTION('ref_axis',(-1.,2.22044604925031E-16,0.));
#13303=DIRECTION('center_axis',(-1.75415237890772E-14,1.,0.));
#13304=DIRECTION('ref_axis',(0.,0.,1.));
#13305=DIRECTION('center_axis',(0.,0.,1.));
#13306=DIRECTION('ref_axis',(-0.707106781186547,0.707106781186548,0.));
#13307=DIRECTION('',(0.,0.,-1.));
#13308=DIRECTION('',(0.,0.,1.));
#13309=DIRECTION('center_axis',(-1.,2.22044604925031E-16,0.));
#13310=DIRECTION('ref_axis',(0.,0.,-1.));
#13311=DIRECTION('center_axis',(0.,0.,-1.));
#13312=DIRECTION('ref_axis',(1.,-2.22044604925031E-16,0.));
#13313=DIRECTION('center_axis',(1.,-2.22044604925031E-16,0.));
#13314=DIRECTION('ref_axis',(1.57009245868377E-16,0.707106781186546,0.707106781186549));
#13315=DIRECTION('center_axis',(-2.22044604925031E-16,-1.,0.));
#13316=DIRECTION('ref_axis',(0.,0.,-1.));
#13317=DIRECTION('center_axis',(0.,0.,1.));
#13318=DIRECTION('ref_axis',(0.707106781186554,-0.707106781186541,0.));
#13319=DIRECTION('',(0.,0.,1.));
#13320=DIRECTION('center_axis',(0.408248290463854,-0.408248290463854,-0.816496580927736));
#13321=DIRECTION('ref_axis',(0.577350269189616,-0.577350269189645,0.577350269189616));
#13322=DIRECTION('center_axis',(1.,-2.22044604925031E-16,0.));
#13323=DIRECTION('ref_axis',(-2.22044604925031E-16,-1.,0.));
#13324=DIRECTION('center_axis',(0.,0.,1.));
#13325=DIRECTION('ref_axis',(1.,-2.22044604925031E-16,0.));
#13326=DIRECTION('center_axis',(1.75415237890772E-14,-1.,0.));
#13327=DIRECTION('ref_axis',(0.,0.,1.));
#13328=DIRECTION('center_axis',(1.,-2.22044604925031E-16,0.));
#13329=DIRECTION('ref_axis',(0.,0.,1.));
#13330=DIRECTION('center_axis',(-2.22044604925031E-16,-1.,0.));
#13331=DIRECTION('ref_axis',(-1.,2.22044604925031E-16,0.));
#13332=DIRECTION('center_axis',(-1.,2.22044604925031E-16,0.));
#13333=DIRECTION('ref_axis',(1.57009245868378E-16,0.707106781186549,0.707106781186546));
#13334=DIRECTION('center_axis',(0.,0.,-1.));
#13335=DIRECTION('ref_axis',(-2.22044604925031E-16,-1.,0.));
#13336=DIRECTION('center_axis',(-0.408248290463875,0.816496580927721,0.408248290463861));
#13337=DIRECTION('ref_axis',(-0.577350269189635,-0.577350269189635,0.577350269189607));
#13338=DIRECTION('center_axis',(-2.22044604925031E-16,-1.,0.));
#13339=DIRECTION('ref_axis',(-1.,2.22044604925031E-16,0.));
#13340=DIRECTION('center_axis',(0.,0.,1.));
#13341=DIRECTION('ref_axis',(-2.22044604925031E-16,-1.,0.));
#13342=DIRECTION('center_axis',(-1.,2.22044604925031E-16,0.));
#13343=DIRECTION('ref_axis',(0.,0.,1.));
#13344=DIRECTION('center_axis',(-0.408248290463854,0.408248290463854,-0.816496580927736));
#13345=DIRECTION('ref_axis',(0.577350269189616,-0.577350269189645,-0.577350269189616));
#13346=DIRECTION('center_axis',(-2.22044604925031E-16,-1.,1.77635683940026E-14));
#13347=DIRECTION('ref_axis',(1.,-2.22044604925031E-16,0.));
#13348=DIRECTION('center_axis',(0.,0.,-1.));
#13349=DIRECTION('ref_axis',(-2.22044604925031E-16,-1.,0.));
#13350=DIRECTION('center_axis',(-2.22044604925031E-16,-1.,0.));
#13351=DIRECTION('ref_axis',(0.707106781186554,-1.57009245868379E-16,-0.707106781186541));
#13352=DIRECTION('',(-2.22044604925031E-16,-1.,0.));
#13353=DIRECTION('center_axis',(0.408248290463865,0.816496580927731,-0.408248290463851));
#13354=DIRECTION('ref_axis',(0.577350269189626,-0.577350269189626,-0.577350269189626));
#13355=DIRECTION('center_axis',(0.,0.,-1.));
#13356=DIRECTION('ref_axis',(-2.22044604925031E-16,-1.,0.));
#13357=DIRECTION('center_axis',(1.,-2.22044604925031E-16,0.));
#13358=DIRECTION('ref_axis',(0.,0.,-1.));
#13359=DIRECTION('center_axis',(-2.22044604925031E-16,-1.,1.77635683940026E-14));
#13360=DIRECTION('ref_axis',(1.,-2.22044604925031E-16,0.));
#13361=DIRECTION('center_axis',(0.408248290463854,0.408248290463854,-0.816496580927736));
#13362=DIRECTION('ref_axis',(-0.577350269189616,-0.577350269189645,-0.577350269189616));
#13363=DIRECTION('center_axis',(0.,0.,-1.));
#13364=DIRECTION('ref_axis',(-1.,2.22044604925031E-16,0.));
#13365=DIRECTION('center_axis',(-2.22044604925031E-16,-1.,0.));
#13366=DIRECTION('ref_axis',(0.,0.,-1.));
#13367=DIRECTION('center_axis',(0.408248290463858,0.408248290463858,-0.816496580927731));
#13368=DIRECTION('ref_axis',(-0.577350269189631,-0.577350269189631,-0.577350269189616));
#13369=DIRECTION('center_axis',(0.,0.,-1.));
#13370=DIRECTION('ref_axis',(-1.,2.22044604925031E-16,0.));
#13371=DIRECTION('center_axis',(-2.22044604925031E-16,-1.,0.));
#13372=DIRECTION('ref_axis',(0.,0.,-1.));
#13373=DIRECTION('center_axis',(-1.,2.22044604925031E-16,0.));
#13374=DIRECTION('ref_axis',(-2.22044604925031E-16,-1.,0.));
#13375=DIRECTION('center_axis',(-1.,2.22044604925031E-16,0.));
#13376=DIRECTION('ref_axis',(0.,0.,-1.));
#13377=DIRECTION('center_axis',(0.,0.,-1.));
#13378=DIRECTION('ref_axis',(1.,-2.22044604925031E-16,0.));
#13379=DIRECTION('center_axis',(1.,-2.22044604925031E-16,0.));
#13380=DIRECTION('ref_axis',(1.57009245868377E-16,0.707106781186548,0.707106781186548));
#13381=DIRECTION('center_axis',(-2.22044604925031E-16,-1.,0.));
#13382=DIRECTION('ref_axis',(0.,0.,-1.));
#13383=DIRECTION('center_axis',(0.,0.,1.));
#13384=DIRECTION('ref_axis',(0.707106781186547,-0.707106781186548,0.));
#13385=DIRECTION('',(0.,0.,1.));
#13386=DIRECTION('center_axis',(2.22044604925031E-16,1.,0.));
#13387=DIRECTION('ref_axis',(0.707106781186554,-1.57009245868379E-16,-0.707106781186541));
#13388=DIRECTION('',(-2.22044604925031E-16,-1.,0.));
#13389=DIRECTION('center_axis',(1.,-2.22044604925031E-16,0.));
#13390=DIRECTION('ref_axis',(0.,0.,1.));
#13391=DIRECTION('center_axis',(-2.22044604925031E-16,-1.,0.));
#13392=DIRECTION('ref_axis',(-1.,2.22044604925031E-16,0.));
#13393=DIRECTION('center_axis',(-1.,2.22044604925031E-16,0.));
#13394=DIRECTION('ref_axis',(1.57009245868377E-16,0.707106781186548,0.707106781186548));
#13395=DIRECTION('center_axis',(0.,0.,-1.));
#13396=DIRECTION('ref_axis',(-2.22044604925031E-16,-1.,0.));
#13397=DIRECTION('center_axis',(-2.22044604925031E-16,-1.,0.));
#13398=DIRECTION('ref_axis',(-0.707106781186554,1.57009245868379E-16,-0.707106781186541));
#13399=DIRECTION('',(2.22044604925031E-16,1.,0.));
#13400=DIRECTION('center_axis',(0.,0.,-1.));
#13401=DIRECTION('ref_axis',(-0.707106781186548,-0.707106781186547,0.));
#13402=DIRECTION('',(0.,0.,-1.));
#13403=DIRECTION('center_axis',(1.,-2.22044604925031E-16,0.));
#13404=DIRECTION('ref_axis',(-1.57009245868376E-16,-0.707106781186541,-0.707106781186554));
#13405=DIRECTION('',(-1.,2.22044604925031E-16,0.));
#13406=DIRECTION('center_axis',(0.,0.,1.));
#13407=DIRECTION('ref_axis',(-0.707106781186548,-0.707106781186547,0.));
#13408=DIRECTION('',(0.,0.,-1.));
#13409=DIRECTION('',(0.,0.,1.));
#13410=DIRECTION('center_axis',(2.22044604925031E-16,1.,0.));
#13411=DIRECTION('ref_axis',(-0.707106781186554,1.57009245868379E-16,-0.707106781186541));
#13412=DIRECTION('',(2.22044604925031E-16,1.,0.));
#13413=DIRECTION('center_axis',(-1.,2.22044604925031E-16,0.));
#13414=DIRECTION('ref_axis',(-1.57009245868376E-16,-0.707106781186541,-0.707106781186554));
#13415=DIRECTION('',(-1.,2.22044604925031E-16,0.));
#13416=DIRECTION('center_axis',(0.,0.,1.));
#13417=DIRECTION('ref_axis',(0.707106781186547,-0.707106781186548,0.));
#13418=DIRECTION('',(0.,0.,-1.));
#13419=DIRECTION('',(0.,0.,1.));
#13420=DIRECTION('center_axis',(1.,-2.22044604925031E-16,0.));
#13421=DIRECTION('ref_axis',(-1.57009245868376E-16,-0.707106781186541,0.707106781186554));
#13422=DIRECTION('',(-1.,2.22044604925031E-16,0.));
#13423=DIRECTION('',(1.,-2.22044604925031E-16,0.));
#13424=DIRECTION('center_axis',(-2.22044604925031E-16,-1.,0.));
#13425=DIRECTION('ref_axis',(-0.707106781186554,1.57009245868379E-16,0.707106781186541));
#13426=DIRECTION('',(2.22044604925031E-16,1.,0.));
#13427=DIRECTION('',(-2.22044604925031E-16,-1.,0.));
#13428=DIRECTION('center_axis',(0.,0.,-1.));
#13429=DIRECTION('ref_axis',(-0.707106781186554,-0.707106781186541,0.));
#13430=DIRECTION('',(0.,0.,-1.));
#13431=DIRECTION('center_axis',(2.22044604925031E-16,1.,0.));
#13432=DIRECTION('ref_axis',(0.707106781186554,-1.57009245868379E-16,0.707106781186541));
#13433=DIRECTION('',(-2.22044604925031E-16,-1.,0.));
#13434=DIRECTION('',(2.22044604925031E-16,1.,0.));
#13435=DIRECTION('center_axis',(-1.,2.22044604925031E-16,0.));
#13436=DIRECTION('ref_axis',(1.57009245868376E-16,0.707106781186541,0.707106781186554));
#13437=DIRECTION('',(1.,-2.22044604925031E-16,0.));
#13438=DIRECTION('',(-1.,2.22044604925031E-16,0.));
#13439=DIRECTION('center_axis',(2.22044604925031E-16,1.,0.));
#13440=DIRECTION('ref_axis',(-0.707106781186553,1.57009245868379E-16,-0.707106781186542));
#13441=DIRECTION('',(2.22044604925031E-16,1.,0.));
#13442=DIRECTION('center_axis',(-1.,2.22044604925031E-16,0.));
#13443=DIRECTION('ref_axis',(-1.57009245868377E-16,-0.707106781186546,-0.707106781186549));
#13444=DIRECTION('',(-1.,2.22044604925031E-16,0.));
#13445=DIRECTION('center_axis',(-1.,2.22044604925031E-16,0.));
#13446=DIRECTION('ref_axis',(1.57009245868376E-16,0.707106781186541,-0.707106781186554));
#13447=DIRECTION('',(1.,-2.22044604925031E-16,0.));
#13448=DIRECTION('center_axis',(0.,0.,1.));
#13449=DIRECTION('ref_axis',(-0.707106781186554,0.707106781186541,0.));
#13450=DIRECTION('',(0.,0.,1.));
#13451=DIRECTION('center_axis',(-1.,2.22044604925031E-16,0.));
#13452=DIRECTION('ref_axis',(-2.05142465794791E-16,-0.923879532511288,0.382683432365088));
#13453=DIRECTION('',(-1.,2.22044604925031E-16,0.));
#13454=DIRECTION('center_axis',(2.22044604925031E-16,1.,0.));
#13455=DIRECTION('ref_axis',(-0.707106781186554,1.57009245868379E-16,-0.707106781186541));
#13456=DIRECTION('',(2.22044604925031E-16,1.,0.));
#13457=DIRECTION('center_axis',(1.57009245868377E-16,0.707106781186548,
-0.707106781186548));
#13458=DIRECTION('ref_axis',(0.707106781186553,0.499999999999997,0.499999999999996));
#13459=DIRECTION('',(1.57009245868377E-16,0.707106781186548,-0.707106781186548));
#13460=DIRECTION('center_axis',(-1.,2.22044604925031E-16,0.));
#13461=DIRECTION('ref_axis',(2.05142465794791E-16,0.923879532511283,-0.382683432365098));
#13462=DIRECTION('',(-1.,2.22044604925031E-16,0.));
#13463=DIRECTION('',(1.,-2.22044604925031E-16,0.));
#13464=DIRECTION('center_axis',(-1.,2.22044604925031E-16,0.));
#13465=DIRECTION('ref_axis',(-2.22044604925031E-16,-1.,0.));
#13466=DIRECTION('center_axis',(1.57009245868377E-16,0.707106781186548,
0.707106781186548));
#13467=DIRECTION('ref_axis',(1.57009245868377E-16,0.707106781186548,-0.707106781186548));
#13468=DIRECTION('center_axis',(2.22044604925031E-16,1.,0.));
#13469=DIRECTION('ref_axis',(-1.,2.22044604925031E-16,0.));
#13470=DIRECTION('center_axis',(-2.22044604925031E-16,-1.,0.));
#13471=DIRECTION('ref_axis',(0.,0.,1.));
#13472=DIRECTION('center_axis',(-2.22044604925031E-16,-1.,0.));
#13473=DIRECTION('ref_axis',(1.,-2.22044604925031E-16,0.));
#13474=DIRECTION('center_axis',(0.,0.,1.));
#13475=DIRECTION('ref_axis',(-2.22044604925031E-16,-1.,0.));
#13476=DIRECTION('center_axis',(-2.22044604925031E-16,-1.,0.));
#13477=DIRECTION('ref_axis',(0.,0.,1.));
#13478=DIRECTION('center_axis',(0.,0.,-1.));
#13479=DIRECTION('ref_axis',(-2.22044604925031E-16,-1.,0.));
#13480=DIRECTION('center_axis',(1.,-2.22044604925031E-16,0.));
#13481=DIRECTION('ref_axis',(2.22044604925031E-16,1.,0.));
#13482=DIRECTION('axis',(0.,0.,1.));
#13483=DIRECTION('refdir',(1.,0.,0.));
#13484=DIRECTION('center_axis',(1.,0.,0.));
#13485=DIRECTION('ref_axis',(0.,0.707106781186519,-0.707106781186576));
#13486=DIRECTION('center_axis',(1.,0.,0.));
#13487=DIRECTION('ref_axis',(0.,0.,-1.));
#13488=DIRECTION('',(1.,0.,0.));
#13489=DIRECTION('center_axis',(-1.,0.,0.));
#13490=DIRECTION('ref_axis',(0.,1.,0.));
#13491=DIRECTION('',(-1.,0.,0.));
#13492=DIRECTION('center_axis',(0.,0.,1.));
#13493=DIRECTION('ref_axis',(1.,0.,0.));
#13494=DIRECTION('center_axis',(1.,0.,0.));
#13495=DIRECTION('ref_axis',(0.,-1.,0.));
#13496=DIRECTION('center_axis',(0.,0.,-1.));
#13497=DIRECTION('ref_axis',(1.,0.,0.));
#13498=DIRECTION('center_axis',(0.,0.,1.));
#13499=DIRECTION('ref_axis',(1.,0.,0.));
#13500=DIRECTION('center_axis',(-1.,0.,0.));
#13501=DIRECTION('ref_axis',(0.,-0.707106781186561,-0.707106781186534));
#13502=DIRECTION('center_axis',(1.,0.,0.));
#13503=DIRECTION('ref_axis',(0.,-1.,0.));
#13504=DIRECTION('',(1.,0.,0.));
#13505=DIRECTION('',(-1.,0.,0.));
#13506=DIRECTION('center_axis',(0.,0.,1.));
#13507=DIRECTION('ref_axis',(-1.,0.,0.));
#13508=DIRECTION('center_axis',(0.,0.,-1.));
#13509=DIRECTION('ref_axis',(-1.,0.,0.));
#13510=DIRECTION('center_axis',(0.,0.,1.));
#13511=DIRECTION('ref_axis',(-1.,0.,0.));
#13512=DIRECTION('center_axis',(0.,0.,-1.));
#13513=DIRECTION('ref_axis',(0.,-1.,0.));
#13514=DIRECTION('',(0.,0.,-1.));
#13515=DIRECTION('center_axis',(0.,0.,-1.));
#13516=DIRECTION('ref_axis',(1.,0.,0.));
#13517=DIRECTION('',(0.,0.,-1.));
#13518=DIRECTION('center_axis',(0.,-1.,0.));
#13519=DIRECTION('ref_axis',(-1.,0.,0.));
#13520=DIRECTION('',(0.,0.,-1.));
#13521=DIRECTION('',(-1.,0.,0.));
#13522=DIRECTION('center_axis',(0.,0.,-1.));
#13523=DIRECTION('ref_axis',(-1.,0.,0.));
#13524=DIRECTION('',(1.,0.,0.));
#13525=DIRECTION('',(0.,-1.,0.));
#13526=DIRECTION('',(-1.,0.,0.));
#13527=DIRECTION('',(0.,1.,0.));
#13528=DIRECTION('center_axis',(0.,-1.,0.));
#13529=DIRECTION('ref_axis',(0.,0.,-1.));
#13530=DIRECTION('center_axis',(1.,0.,0.));
#13531=DIRECTION('ref_axis',(0.,0.,-1.));
#13532=DIRECTION('center_axis',(0.,-1.,0.));
#13533=DIRECTION('ref_axis',(-1.,0.,0.));
#13534=DIRECTION('center_axis',(0.,0.,-1.));
#13535=DIRECTION('ref_axis',(0.,1.,0.));
#13536=DIRECTION('center_axis',(0.,1.,0.));
#13537=DIRECTION('ref_axis',(-0.70710678118654,0.,0.707106781186555));
#13538=DIRECTION('center_axis',(-0.816496580927734,-0.408248290463867,0.408248290463843));
#13539=DIRECTION('ref_axis',(-0.577350269189598,0.577350269189645,-0.577350269189634));
#13540=DIRECTION('center_axis',(-1.,0.,0.));
#13541=DIRECTION('ref_axis',(0.,0.,-1.));
#13542=DIRECTION('center_axis',(0.,1.,0.));
#13543=DIRECTION('ref_axis',(-1.,0.,0.));
#13544=DIRECTION('center_axis',(-9.25185853854317E-16,0.,-1.));
#13545=DIRECTION('ref_axis',(0.,1.,0.));
#13546=DIRECTION('center_axis',(0.,-1.,0.));
#13547=DIRECTION('ref_axis',(0.,0.,-1.));
#13548=DIRECTION('center_axis',(0.,-1.,0.));
#13549=DIRECTION('ref_axis',(-0.70710678118654,0.,0.707106781186555));
#13550=DIRECTION('center_axis',(0.,0.,-1.));
#13551=DIRECTION('ref_axis',(1.,0.,0.));
#13552=DIRECTION('center_axis',(-5.92118946466763E-14,1.,0.));
#13553=DIRECTION('ref_axis',(0.,0.,1.));
#13554=DIRECTION('center_axis',(1.,0.,0.));
#13555=DIRECTION('ref_axis',(0.,-1.,0.));
#13556=DIRECTION('center_axis',(0.,0.,-1.));
#13557=DIRECTION('ref_axis',(0.707106781186547,-0.707106781186547,0.));
#13558=DIRECTION('',(0.,0.,1.));
#13559=DIRECTION('',(0.,0.,-1.));
#13560=DIRECTION('center_axis',(0.707106781186576,0.,0.707106781186519));
#13561=DIRECTION('ref_axis',(-0.707106781186519,0.,0.707106781186576));
#13562=DIRECTION('center_axis',(-0.827465426020362,0.538877990790925,-0.157833709270471));
#13563=DIRECTION('ref_axis',(0.561516668266355,0.794104487760816,-0.232587819494453));
#13564=DIRECTION('center_axis',(0.707106781186544,-3.663549070262E-14,-0.707106781186551));
#13565=DIRECTION('ref_axis',(0.707106781186551,0.,0.707106781186544));
#13566=DIRECTION('center_axis',(0.,1.,0.));
#13567=DIRECTION('ref_axis',(0.,0.,-1.));
#13568=DIRECTION('center_axis',(1.,0.,-2.96059473233375E-14));
#13569=DIRECTION('ref_axis',(0.,1.,0.));
#13570=DIRECTION('center_axis',(0.408248290463871,0.408248290463824,-0.816496580927742));
#13571=DIRECTION('ref_axis',(-0.577350269189681,-0.577350269189586,-0.57735026918961));
#13572=DIRECTION('center_axis',(0.,-1.,0.));
#13573=DIRECTION('ref_axis',(0.,0.,-1.));
#13574=DIRECTION('center_axis',(-1.,0.,5.9211894646675E-14));
#13575=DIRECTION('ref_axis',(0.,-1.,0.));
#13576=DIRECTION('center_axis',(0.,-9.25185853854317E-16,-1.));
#13577=DIRECTION('ref_axis',(-1.,0.,0.));
#13578=DIRECTION('center_axis',(-1.,0.,0.));
#13579=DIRECTION('ref_axis',(0.,-0.707106781186519,-0.707106781186576));
#13580=DIRECTION('',(-1.,0.,0.));
#13581=DIRECTION('',(1.,0.,0.));
#13582=DIRECTION('center_axis',(-0.408248290463863,0.408248290463816,-0.81649658092775));
#13583=DIRECTION('ref_axis',(-0.577350269189665,0.577350269189618,0.577350269189594));
#13584=DIRECTION('center_axis',(0.,0.,1.));
#13585=DIRECTION('ref_axis',(-1.,0.,0.));
#13586=DIRECTION('center_axis',(0.,1.,0.));
#13587=DIRECTION('ref_axis',(0.,0.,1.));
#13588=DIRECTION('center_axis',(-1.,0.,5.9211894646675E-14));
#13589=DIRECTION('ref_axis',(0.,1.,0.));
#13590=DIRECTION('center_axis',(-0.827465426020388,-0.538877990790895,-0.157833709270442));
#13591=DIRECTION('ref_axis',(0.561516668266318,-0.794104487760845,-0.232587819494444));
#13592=DIRECTION('center_axis',(0.,-1.,0.));
#13593=DIRECTION('ref_axis',(0.707106781186544,0.,0.707106781186551));
#13594=DIRECTION('center_axis',(0.70710678118657,0.,-0.707106781186525));
#13595=DIRECTION('ref_axis',(0.,-1.,0.));
#13596=DIRECTION('center_axis',(1.,2.96059473233364E-14,0.));
#13597=DIRECTION('ref_axis',(0.,0.,-1.));
#13598=DIRECTION('center_axis',(0.182143211721525,-0.8794652240646,0.439732612032324));
#13599=DIRECTION('ref_axis',(0.336556770590774,0.475963149478001,0.812519920068728));
#13600=DIRECTION('center_axis',(1.,0.,0.));
#13601=DIRECTION('ref_axis',(0.,0.,1.));
#13602=DIRECTION('center_axis',(0.,1.,0.));
#13603=DIRECTION('ref_axis',(0.707106781186551,0.,0.707106781186544));
#13604=DIRECTION('center_axis',(-0.70710678118654,0.,0.707106781186555));
#13605=DIRECTION('ref_axis',(0.,1.,0.));
#13606=DIRECTION('center_axis',(-0.408248290463908,-0.408248290463861,-0.816496580927704));
#13607=DIRECTION('ref_axis',(-0.577350269189642,-0.577350269189594,0.577350269189642));
#13608=DIRECTION('center_axis',(0.,-1.,5.9211894646675E-14));
#13609=DIRECTION('ref_axis',(-1.,0.,0.));
#13610=DIRECTION('center_axis',(0.,0.,1.));
#13611=DIRECTION('ref_axis',(0.,-1.,0.));
#13612=DIRECTION('center_axis',(-1.,0.,0.));
#13613=DIRECTION('ref_axis',(0.,0.,1.));
#13614=DIRECTION('center_axis',(0.,0.,1.));
#13615=DIRECTION('ref_axis',(-0.707106781186589,-0.707106781186506,0.));
#13616=DIRECTION('',(0.,0.,-1.));
#13617=DIRECTION('',(0.,0.,1.));
#13618=DIRECTION('center_axis',(-0.182143211721517,-0.879465224064606,-0.439732612032315));
#13619=DIRECTION('ref_axis',(0.336556770590767,-0.475963149477992,0.812519920068736));
#13620=DIRECTION('center_axis',(0.,-1.,0.));
#13621=DIRECTION('ref_axis',(0.,0.,1.));
#13622=DIRECTION('center_axis',(1.,0.,0.));
#13623=DIRECTION('ref_axis',(0.,-1.,0.));
#13624=DIRECTION('center_axis',(-0.70710678118654,0.,0.707106781186555));
#13625=DIRECTION('ref_axis',(0.707106781186555,0.,0.70710678118654));
#13626=DIRECTION('center_axis',(-1.,0.,0.));
#13627=DIRECTION('ref_axis',(0.,-0.707106781186558,0.707106781186537));
#13628=DIRECTION('',(1.,0.,0.));
#13629=DIRECTION('',(-1.,0.,0.));
#13630=DIRECTION('center_axis',(-0.707106781186547,0.,0.707106781186548));
#13631=DIRECTION('ref_axis',(0.499999999999997,-0.707106781186559,0.499999999999986));
#13632=DIRECTION('',(0.707106781186547,0.,-0.707106781186548));
#13633=DIRECTION('',(-0.707106781186547,0.,0.707106781186548));
#13634=DIRECTION('center_axis',(0.,1.,0.));
#13635=DIRECTION('ref_axis',(0.382683432365094,0.,0.923879532511285));
#13636=DIRECTION('',(0.,-1.,0.));
#13637=DIRECTION('',(0.,1.,0.));
#13638=DIRECTION('center_axis',(0.,1.,0.));
#13639=DIRECTION('ref_axis',(-0.707106781186558,0.,0.707106781186537));
#13640=DIRECTION('',(0.,-1.,0.));
#13641=DIRECTION('',(0.,1.,0.));
#13642=DIRECTION('center_axis',(0.707106781186547,0.,-0.707106781186548));
#13643=DIRECTION('ref_axis',(0.499999999999997,0.707106781186559,0.499999999999986));
#13644=DIRECTION('',(-0.707106781186547,0.,0.707106781186548));
#13645=DIRECTION('',(0.707106781186547,0.,-0.707106781186548));
#13646=DIRECTION('center_axis',(1.,0.,0.));
#13647=DIRECTION('ref_axis',(0.,0.707106781186558,0.707106781186537));
#13648=DIRECTION('',(-1.,0.,0.));
#13649=DIRECTION('',(1.,0.,0.));
#13650=DIRECTION('center_axis',(1.,0.,0.));
#13651=DIRECTION('ref_axis',(0.,-0.707106781186561,-0.707106781186534));
#13652=DIRECTION('',(-1.,0.,0.));
#13653=DIRECTION('center_axis',(0.,1.,0.));
#13654=DIRECTION('ref_axis',(0.923879532511297,0.,-0.382683432365066));
#13655=DIRECTION('',(0.,-1.,0.));
#13656=DIRECTION('center_axis',(0.,0.,1.));
#13657=DIRECTION('ref_axis',(-0.707106781186506,0.707106781186589,0.));
#13658=DIRECTION('',(0.,0.,-1.));
#13659=DIRECTION('',(0.,0.,1.));
#13660=DIRECTION('center_axis',(0.,1.,0.));
#13661=DIRECTION('ref_axis',(-0.707106781186519,0.,-0.707106781186576));
#13662=DIRECTION('',(0.,-1.,0.));
#13663=DIRECTION('',(0.,1.,0.));
#13664=DIRECTION('center_axis',(-1.,0.,0.));
#13665=DIRECTION('ref_axis',(0.,0.707106781186561,-0.707106781186534));
#13666=DIRECTION('',(1.,0.,0.));
#13667=DIRECTION('center_axis',(0.,1.,0.));
#13668=DIRECTION('ref_axis',(-0.707106781186519,0.,0.707106781186576));
#13669=DIRECTION('',(0.,1.,0.));
#13670=DIRECTION('center_axis',(-1.,0.,0.));
#13671=DIRECTION('ref_axis',(0.,0.707106781186561,-0.707106781186534));
#13672=DIRECTION('',(-1.,0.,0.));
#13673=DIRECTION('',(1.,0.,0.));
#13674=DIRECTION('center_axis',(-0.707106781186555,0.,-0.70710678118654));
#13675=DIRECTION('ref_axis',(0.70710678118654,0.,-0.707106781186555));
#13676=DIRECTION('center_axis',(0.,0.,-1.));
#13677=DIRECTION('ref_axis',(0.707106781186506,0.707106781186589,0.));
#13678=DIRECTION('',(0.,0.,1.));
#13679=DIRECTION('',(0.,0.,-1.));
#13680=DIRECTION('center_axis',(1.,0.,0.));
#13681=DIRECTION('ref_axis',(0.,0.,-1.));
#13682=DIRECTION('',(0.,1.,0.));
#13683=DIRECTION('center_axis',(0.,1.,0.));
#13684=DIRECTION('ref_axis',(1.,0.,0.));
#13685=DIRECTION('center_axis',(-1.,0.,0.));
#13686=DIRECTION('ref_axis',(0.,0.,1.));
#13687=DIRECTION('center_axis',(0.,0.,1.));
#13688=DIRECTION('ref_axis',(1.,0.,0.));
#13689=DIRECTION('',(1.,0.,0.));
#13690=DIRECTION('center_axis',(0.,0.,1.));
#13691=DIRECTION('ref_axis',(-1.,0.,0.));
#13692=DIRECTION('',(-1.,0.,0.));
#13693=DIRECTION('center_axis',(0.,0.,1.));
#13694=DIRECTION('ref_axis',(1.,0.,0.));
#13695=DIRECTION('center_axis',(0.707106781186548,0.,0.707106781186547));
#13696=DIRECTION('ref_axis',(0.707106781186547,0.,-0.707106781186548));
#13697=DIRECTION('center_axis',(0.,1.,0.));
#13698=DIRECTION('ref_axis',(0.,0.,1.));
#13699=DIRECTION('center_axis',(-1.,0.,0.));
#13700=DIRECTION('ref_axis',(0.,0.707106781186516,0.707106781186579));
#13701=DIRECTION('center_axis',(-1.,0.,0.));
#13702=DIRECTION('ref_axis',(0.,0.,1.));
#13703=DIRECTION('center_axis',(1.,0.,0.));
#13704=DIRECTION('ref_axis',(0.,1.,0.));
#13705=DIRECTION('center_axis',(0.,0.,-1.));
#13706=DIRECTION('ref_axis',(-1.,0.,0.));
#13707=DIRECTION('center_axis',(-1.,0.,0.));
#13708=DIRECTION('ref_axis',(0.,-1.,0.));
#13709=DIRECTION('center_axis',(0.,0.,-1.));
#13710=DIRECTION('ref_axis',(-1.,0.,0.));
#13711=DIRECTION('center_axis',(1.,0.,0.));
#13712=DIRECTION('ref_axis',(0.,-0.707106781186558,0.707106781186537));
#13713=DIRECTION('center_axis',(-1.,0.,0.));
#13714=DIRECTION('ref_axis',(0.,-1.,0.));
#13715=DIRECTION('',(1.,0.,0.));
#13716=DIRECTION('center_axis',(0.,0.,-1.));
#13717=DIRECTION('ref_axis',(1.,0.,0.));
#13718=DIRECTION('center_axis',(0.,0.,-1.));
#13719=DIRECTION('ref_axis',(0.,1.,0.));
#13720=DIRECTION('',(0.,0.,-1.));
#13721=DIRECTION('center_axis',(0.,1.,0.));
#13722=DIRECTION('ref_axis',(1.,0.,0.));
#13723=DIRECTION('center_axis',(0.,0.,-1.));
#13724=DIRECTION('ref_axis',(-1.,0.,0.));
#13725=DIRECTION('axis',(0.,0.,1.));
#13726=DIRECTION('refdir',(1.,0.,0.));
#13727=DIRECTION('center_axis',(-1.,2.22044604925031E-16,0.));
#13728=DIRECTION('ref_axis',(-2.22044604925031E-16,-1.,0.));
#13729=DIRECTION('center_axis',(-1.,2.22044604925031E-16,0.));
#13730=DIRECTION('ref_axis',(-2.22044604925031E-16,-1.,0.));
#13731=DIRECTION('center_axis',(-1.,2.22044604925031E-16,0.));
#13732=DIRECTION('ref_axis',(-2.22044604925031E-16,-1.,0.));
#13733=DIRECTION('center_axis',(1.,-2.22044604925031E-16,0.));
#13734=DIRECTION('ref_axis',(-2.22044604925031E-16,-1.,0.));
#13735=DIRECTION('center_axis',(1.,-2.22044604925031E-16,0.));
#13736=DIRECTION('ref_axis',(-2.22044604925031E-16,-1.,0.));
#13737=DIRECTION('',(0.707106781186547,0.707106781186549,-8.65956056235495E-17));
#13738=DIRECTION('center_axis',(-1.,2.22044604925031E-16,0.));
#13739=DIRECTION('ref_axis',(-2.22044604925031E-16,-1.,0.));
#13740=DIRECTION('center_axis',(-1.,2.22044604925031E-16,0.));
#13741=DIRECTION('ref_axis',(-2.22044604925031E-16,-1.,0.));
#13742=DIRECTION('',(1.,-2.22044604925031E-16,0.));
#13743=DIRECTION('center_axis',(1.,-2.22044604925031E-16,0.));
#13744=DIRECTION('ref_axis',(-2.22044604925031E-16,-1.,0.));
#13745=DIRECTION('center_axis',(-1.,2.22044604925031E-16,0.));
#13746=DIRECTION('ref_axis',(-2.22044604925031E-16,-1.,0.));
#13747=DIRECTION('center_axis',(-1.,2.22044604925031E-16,0.));
#13748=DIRECTION('ref_axis',(-2.22044604925031E-16,-1.,0.));
#13749=DIRECTION('',(0.707106781186546,-0.707106781186549,8.65956056235495E-17));
#13750=DIRECTION('center_axis',(-1.,2.22044604925031E-16,0.));
#13751=DIRECTION('ref_axis',(-2.22044604925031E-16,-1.,0.));
#13752=DIRECTION('',(1.,-2.22044604925031E-16,0.));
#13753=DIRECTION('center_axis',(-1.,2.22044604925031E-16,0.));
#13754=DIRECTION('ref_axis',(-2.22044604925031E-16,-1.,0.));
#13755=DIRECTION('center_axis',(-1.,2.22044604925031E-16,0.));
#13756=DIRECTION('ref_axis',(-2.22044604925031E-16,-1.,0.));
#13757=DIRECTION('axis',(0.,0.,1.));
#13758=DIRECTION('refdir',(1.,0.,0.));
#13759=DIRECTION('center_axis',(1.,0.,0.));
#13760=DIRECTION('ref_axis',(0.,0.707106781186519,-0.707106781186576));
#13761=DIRECTION('center_axis',(1.,0.,0.));
#13762=DIRECTION('ref_axis',(0.,0.,-1.));
#13763=DIRECTION('',(1.,0.,0.));
#13764=DIRECTION('center_axis',(-1.,0.,0.));
#13765=DIRECTION('ref_axis',(0.,1.,0.));
#13766=DIRECTION('',(-1.,0.,0.));
#13767=DIRECTION('center_axis',(0.,0.,1.));
#13768=DIRECTION('ref_axis',(-1.,0.,0.));
#13769=DIRECTION('center_axis',(1.,0.,0.));
#13770=DIRECTION('ref_axis',(0.,-1.,0.));
#13771=DIRECTION('center_axis',(0.,0.,-1.));
#13772=DIRECTION('ref_axis',(-1.,0.,0.));
#13773=DIRECTION('center_axis',(0.,0.,1.));
#13774=DIRECTION('ref_axis',(-1.,0.,0.));
#13775=DIRECTION('center_axis',(-1.,0.,0.));
#13776=DIRECTION('ref_axis',(0.,-0.707106781186561,-0.707106781186534));
#13777=DIRECTION('center_axis',(1.,0.,0.));
#13778=DIRECTION('ref_axis',(0.,-1.,0.));
#13779=DIRECTION('',(1.,0.,0.));
#13780=DIRECTION('',(-1.,0.,0.));
#13781=DIRECTION('center_axis',(0.,0.,1.));
#13782=DIRECTION('ref_axis',(1.,0.,0.));
#13783=DIRECTION('center_axis',(0.,0.,-1.));
#13784=DIRECTION('ref_axis',(1.,0.,0.));
#13785=DIRECTION('center_axis',(0.,0.,1.));
#13786=DIRECTION('ref_axis',(1.,0.,0.));
#13787=DIRECTION('center_axis',(0.,0.,1.));
#13788=DIRECTION('ref_axis',(0.,-1.,0.));
#13789=DIRECTION('',(0.,0.,-1.));
#13790=DIRECTION('center_axis',(0.,0.,1.));
#13791=DIRECTION('ref_axis',(-1.,0.,0.));
#13792=DIRECTION('',(0.,0.,-1.));
#13793=DIRECTION('center_axis',(0.,1.,0.));
#13794=DIRECTION('ref_axis',(1.,0.,0.));
#13795=DIRECTION('',(1.,0.,0.));
#13796=DIRECTION('',(0.,0.,-1.));
#13797=DIRECTION('center_axis',(0.,0.,1.));
#13798=DIRECTION('ref_axis',(1.,0.,0.));
#13799=DIRECTION('',(-1.,0.,0.));
#13800=DIRECTION('',(0.,1.,0.));
#13801=DIRECTION('',(1.,0.,0.));
#13802=DIRECTION('',(0.,-1.,0.));
#13803=DIRECTION('center_axis',(0.,-1.,0.));
#13804=DIRECTION('ref_axis',(0.,0.,-1.));
#13805=DIRECTION('center_axis',(1.,0.,0.));
#13806=DIRECTION('ref_axis',(0.,0.,-1.));
#13807=DIRECTION('center_axis',(0.,-1.,0.));
#13808=DIRECTION('ref_axis',(0.70710678118654,0.,0.707106781186555));
#13809=DIRECTION('center_axis',(0.,0.,1.));
#13810=DIRECTION('ref_axis',(0.,1.,0.));
#13811=DIRECTION('center_axis',(0.,1.,0.));
#13812=DIRECTION('ref_axis',(1.,0.,0.));
#13813=DIRECTION('center_axis',(0.816496580927734,-0.408248290463867,0.408248290463843));
#13814=DIRECTION('ref_axis',(0.577350269189598,0.577350269189645,-0.577350269189634));
#13815=DIRECTION('center_axis',(-1.,0.,0.));
#13816=DIRECTION('ref_axis',(0.,0.,-1.));
#13817=DIRECTION('center_axis',(-9.25185853854317E-16,0.,1.));
#13818=DIRECTION('ref_axis',(0.,1.,0.));
#13819=DIRECTION('center_axis',(0.,-1.,0.));
#13820=DIRECTION('ref_axis',(1.,0.,0.));
#13821=DIRECTION('center_axis',(0.,-1.,0.));
#13822=DIRECTION('ref_axis',(0.,0.,-1.));
#13823=DIRECTION('center_axis',(0.,1.,0.));
#13824=DIRECTION('ref_axis',(0.70710678118654,0.,0.707106781186555));
#13825=DIRECTION('center_axis',(1.,0.,0.));
#13826=DIRECTION('ref_axis',(0.,-1.,0.));
#13827=DIRECTION('center_axis',(-5.92118946466763E-14,-1.,0.));
#13828=DIRECTION('ref_axis',(0.,0.,1.));
#13829=DIRECTION('center_axis',(0.,0.,1.));
#13830=DIRECTION('ref_axis',(-1.,0.,0.));
#13831=DIRECTION('center_axis',(0.,0.,1.));
#13832=DIRECTION('ref_axis',(-0.707106781186547,-0.707106781186547,0.));
#13833=DIRECTION('',(0.,0.,1.));
#13834=DIRECTION('center_axis',(0.707106781186576,0.,-0.707106781186519));
#13835=DIRECTION('ref_axis',(0.707106781186519,0.,0.707106781186576));
#13836=DIRECTION('',(0.,0.,-1.));
#13837=DIRECTION('center_axis',(0.827465426020362,0.538877990790925,-0.157833709270471));
#13838=DIRECTION('ref_axis',(-0.561516668266355,0.794104487760816,-0.232587819494453));
#13839=DIRECTION('center_axis',(0.707106781186544,3.663549070262E-14,0.707106781186551));
#13840=DIRECTION('ref_axis',(-0.707106781186551,0.,0.707106781186544));
#13841=DIRECTION('center_axis',(1.,0.,2.96059473233375E-14));
#13842=DIRECTION('ref_axis',(0.,1.,0.));
#13843=DIRECTION('center_axis',(0.,-1.,0.));
#13844=DIRECTION('ref_axis',(0.,0.,-1.));
#13845=DIRECTION('center_axis',(-0.408248290463871,0.408248290463824,-0.816496580927742));
#13846=DIRECTION('ref_axis',(0.577350269189681,-0.577350269189586,-0.57735026918961));
#13847=DIRECTION('center_axis',(0.,1.,0.));
#13848=DIRECTION('ref_axis',(0.,0.,-1.));
#13849=DIRECTION('center_axis',(0.,9.25185853854317E-16,1.));
#13850=DIRECTION('ref_axis',(1.,0.,0.));
#13851=DIRECTION('center_axis',(-1.,0.,-5.9211894646675E-14));
#13852=DIRECTION('ref_axis',(0.,-1.,0.));
#13853=DIRECTION('center_axis',(-1.,0.,0.));
#13854=DIRECTION('ref_axis',(0.,-0.707106781186519,-0.707106781186576));
#13855=DIRECTION('',(1.,0.,0.));
#13856=DIRECTION('',(-1.,0.,0.));
#13857=DIRECTION('center_axis',(0.408248290463863,0.408248290463816,-0.81649658092775));
#13858=DIRECTION('ref_axis',(0.577350269189665,0.577350269189618,0.577350269189594));
#13859=DIRECTION('center_axis',(0.,0.,-1.));
#13860=DIRECTION('ref_axis',(1.,0.,0.));
#13861=DIRECTION('center_axis',(-1.,0.,-5.9211894646675E-14));
#13862=DIRECTION('ref_axis',(0.,1.,0.));
#13863=DIRECTION('center_axis',(0.,-1.,0.));
#13864=DIRECTION('ref_axis',(0.,0.,1.));
#13865=DIRECTION('center_axis',(0.827465426020388,-0.538877990790895,-0.157833709270442));
#13866=DIRECTION('ref_axis',(-0.561516668266318,-0.794104487760845,-0.232587819494444));
#13867=DIRECTION('center_axis',(0.,1.,0.));
#13868=DIRECTION('ref_axis',(-0.707106781186544,0.,0.707106781186551));
#13869=DIRECTION('center_axis',(1.,-2.96059473233364E-14,0.));
#13870=DIRECTION('ref_axis',(0.,0.,-1.));
#13871=DIRECTION('center_axis',(0.70710678118657,0.,0.707106781186525));
#13872=DIRECTION('ref_axis',(0.,-1.,0.));
#13873=DIRECTION('center_axis',(-0.182143211721525,-0.8794652240646,0.439732612032324));
#13874=DIRECTION('ref_axis',(-0.336556770590774,0.475963149478001,0.812519920068728));
#13875=DIRECTION('center_axis',(1.,0.,0.));
#13876=DIRECTION('ref_axis',(0.,0.,1.));
#13877=DIRECTION('center_axis',(-0.70710678118654,0.,-0.707106781186555));
#13878=DIRECTION('ref_axis',(0.,1.,0.));
#13879=DIRECTION('center_axis',(0.,-1.,0.));
#13880=DIRECTION('ref_axis',(-0.707106781186551,0.,0.707106781186544));
#13881=DIRECTION('center_axis',(0.408248290463908,-0.408248290463861,-0.816496580927704));
#13882=DIRECTION('ref_axis',(0.577350269189642,-0.577350269189594,0.577350269189642));
#13883=DIRECTION('center_axis',(0.,1.,-5.9211894646675E-14));
#13884=DIRECTION('ref_axis',(1.,0.,0.));
#13885=DIRECTION('center_axis',(-1.,0.,0.));
#13886=DIRECTION('ref_axis',(0.,0.,1.));
#13887=DIRECTION('center_axis',(0.,0.,-1.));
#13888=DIRECTION('ref_axis',(0.,-1.,0.));
#13889=DIRECTION('center_axis',(0.,0.,-1.));
#13890=DIRECTION('ref_axis',(0.707106781186589,-0.707106781186506,0.));
#13891=DIRECTION('',(0.,0.,1.));
#13892=DIRECTION('',(0.,0.,-1.));
#13893=DIRECTION('center_axis',(0.182143211721517,-0.879465224064606,-0.439732612032315));
#13894=DIRECTION('ref_axis',(-0.336556770590767,-0.475963149477992,0.812519920068736));
#13895=DIRECTION('center_axis',(0.,1.,0.));
#13896=DIRECTION('ref_axis',(0.,0.,1.));
#13897=DIRECTION('center_axis',(-0.70710678118654,0.,-0.707106781186555));
#13898=DIRECTION('ref_axis',(-0.707106781186555,0.,0.70710678118654));
#13899=DIRECTION('center_axis',(1.,0.,0.));
#13900=DIRECTION('ref_axis',(0.,-1.,0.));
#13901=DIRECTION('center_axis',(-1.,0.,0.));
#13902=DIRECTION('ref_axis',(0.,-0.707106781186558,0.707106781186537));
#13903=DIRECTION('',(1.,0.,0.));
#13904=DIRECTION('',(-1.,0.,0.));
#13905=DIRECTION('center_axis',(-0.707106781186547,0.,-0.707106781186548));
#13906=DIRECTION('ref_axis',(-0.499999999999997,-0.707106781186559,0.499999999999986));
#13907=DIRECTION('',(0.707106781186547,0.,0.707106781186548));
#13908=DIRECTION('',(-0.707106781186547,0.,-0.707106781186548));
#13909=DIRECTION('center_axis',(0.,-1.,0.));
#13910=DIRECTION('ref_axis',(-0.382683432365094,0.,0.923879532511285));
#13911=DIRECTION('',(0.,1.,0.));
#13912=DIRECTION('',(0.,-1.,0.));
#13913=DIRECTION('center_axis',(0.,-1.,0.));
#13914=DIRECTION('ref_axis',(0.707106781186558,0.,0.707106781186537));
#13915=DIRECTION('',(0.,1.,0.));
#13916=DIRECTION('',(0.,-1.,0.));
#13917=DIRECTION('center_axis',(0.707106781186547,0.,0.707106781186548));
#13918=DIRECTION('ref_axis',(-0.499999999999997,0.707106781186559,0.499999999999986));
#13919=DIRECTION('',(-0.707106781186547,0.,-0.707106781186548));
#13920=DIRECTION('',(0.707106781186547,0.,0.707106781186548));
#13921=DIRECTION('center_axis',(1.,0.,0.));
#13922=DIRECTION('ref_axis',(0.,0.707106781186558,0.707106781186537));
#13923=DIRECTION('',(-1.,0.,0.));
#13924=DIRECTION('',(1.,0.,0.));
#13925=DIRECTION('center_axis',(1.,0.,0.));
#13926=DIRECTION('ref_axis',(0.,-0.707106781186561,-0.707106781186534));
#13927=DIRECTION('',(1.,0.,0.));
#13928=DIRECTION('center_axis',(0.,-1.,0.));
#13929=DIRECTION('ref_axis',(-0.923879532511297,0.,-0.382683432365066));
#13930=DIRECTION('',(0.,-1.,0.));
#13931=DIRECTION('center_axis',(0.,0.,-1.));
#13932=DIRECTION('ref_axis',(0.707106781186506,0.707106781186589,0.));
#13933=DIRECTION('',(0.,0.,1.));
#13934=DIRECTION('',(0.,0.,-1.));
#13935=DIRECTION('center_axis',(0.,-1.,0.));
#13936=DIRECTION('ref_axis',(0.707106781186519,0.,-0.707106781186576));
#13937=DIRECTION('',(0.,1.,0.));
#13938=DIRECTION('',(0.,-1.,0.));
#13939=DIRECTION('center_axis',(-1.,0.,0.));
#13940=DIRECTION('ref_axis',(0.,0.707106781186561,-0.707106781186534));
#13941=DIRECTION('',(-1.,0.,0.));
#13942=DIRECTION('center_axis',(0.,-1.,0.));
#13943=DIRECTION('ref_axis',(0.707106781186519,0.,0.707106781186576));
#13944=DIRECTION('',(0.,1.,0.));
#13945=DIRECTION('center_axis',(-1.,0.,0.));
#13946=DIRECTION('ref_axis',(0.,0.707106781186561,-0.707106781186534));
#13947=DIRECTION('',(1.,0.,0.));
#13948=DIRECTION('center_axis',(-0.707106781186555,0.,0.70710678118654));
#13949=DIRECTION('ref_axis',(-0.70710678118654,0.,-0.707106781186555));
#13950=DIRECTION('',(-1.,0.,0.));
#13951=DIRECTION('center_axis',(0.,0.,1.));
#13952=DIRECTION('ref_axis',(-0.707106781186506,0.707106781186589,0.));
#13953=DIRECTION('',(0.,0.,1.));
#13954=DIRECTION('',(0.,0.,-1.));
#13955=DIRECTION('center_axis',(1.,0.,0.));
#13956=DIRECTION('ref_axis',(0.,0.,-1.));
#13957=DIRECTION('',(0.,1.,0.));
#13958=DIRECTION('center_axis',(0.,-1.,0.));
#13959=DIRECTION('ref_axis',(-1.,0.,0.));
#13960=DIRECTION('center_axis',(-1.,0.,0.));
#13961=DIRECTION('ref_axis',(0.,0.,1.));
#13962=DIRECTION('center_axis',(0.,0.,-1.));
#13963=DIRECTION('ref_axis',(-1.,0.,0.));
#13964=DIRECTION('',(-1.,0.,0.));
#13965=DIRECTION('center_axis',(0.,0.,-1.));
#13966=DIRECTION('ref_axis',(-1.,0.,0.));
#13967=DIRECTION('',(1.,0.,0.));
#13968=DIRECTION('center_axis',(0.,0.,-1.));
#13969=DIRECTION('ref_axis',(1.,0.,0.));
#13970=DIRECTION('center_axis',(0.707106781186548,0.,-0.707106781186547));
#13971=DIRECTION('ref_axis',(-0.707106781186547,0.,-0.707106781186548));
#13972=DIRECTION('center_axis',(0.,-1.,0.));
#13973=DIRECTION('ref_axis',(0.,0.,1.));
#13974=DIRECTION('center_axis',(-1.,0.,0.));
#13975=DIRECTION('ref_axis',(0.,0.707106781186516,0.707106781186579));
#13976=DIRECTION('center_axis',(-1.,0.,0.));
#13977=DIRECTION('ref_axis',(0.,0.,1.));
#13978=DIRECTION('center_axis',(1.,0.,0.));
#13979=DIRECTION('ref_axis',(0.,1.,0.));
#13980=DIRECTION('center_axis',(0.,0.,-1.));
#13981=DIRECTION('ref_axis',(1.,0.,0.));
#13982=DIRECTION('center_axis',(-1.,0.,0.));
#13983=DIRECTION('ref_axis',(0.,-1.,0.));
#13984=DIRECTION('center_axis',(0.,0.,1.));
#13985=DIRECTION('ref_axis',(1.,0.,0.));
#13986=DIRECTION('center_axis',(1.,0.,0.));
#13987=DIRECTION('ref_axis',(0.,-0.707106781186558,0.707106781186537));
#13988=DIRECTION('center_axis',(-1.,0.,0.));
#13989=DIRECTION('ref_axis',(0.,-1.,0.));
#13990=DIRECTION('',(-1.,0.,0.));
#13991=DIRECTION('center_axis',(0.,0.,-1.));
#13992=DIRECTION('ref_axis',(-1.,0.,0.));
#13993=DIRECTION('center_axis',(0.,0.,1.));
#13994=DIRECTION('ref_axis',(0.,1.,0.));
#13995=DIRECTION('',(0.,0.,-1.));
#13996=DIRECTION('center_axis',(0.,-1.,0.));
#13997=DIRECTION('ref_axis',(-1.,0.,0.));
#13998=DIRECTION('center_axis',(0.,0.,1.));
#13999=DIRECTION('ref_axis',(1.,0.,0.));
#14000=DIRECTION('axis',(0.,0.,1.));
#14001=DIRECTION('refdir',(1.,0.,0.));
#14002=DIRECTION('center_axis',(-1.,0.,0.));
#14003=DIRECTION('ref_axis',(0.,-0.707106781186519,-0.707106781186576));
#14004=DIRECTION('center_axis',(-1.,0.,0.));
#14005=DIRECTION('ref_axis',(0.,0.,-1.));
#14006=DIRECTION('',(-1.,0.,0.));
#14007=DIRECTION('center_axis',(1.,0.,0.));
#14008=DIRECTION('ref_axis',(0.,-1.,0.));
#14009=DIRECTION('',(1.,0.,0.));
#14010=DIRECTION('center_axis',(0.,0.,1.));
#14011=DIRECTION('ref_axis',(-1.,0.,0.));
#14012=DIRECTION('center_axis',(-1.,0.,0.));
#14013=DIRECTION('ref_axis',(0.,1.,0.));
#14014=DIRECTION('center_axis',(0.,0.,-1.));
#14015=DIRECTION('ref_axis',(-1.,0.,0.));
#14016=DIRECTION('center_axis',(0.,0.,1.));
#14017=DIRECTION('ref_axis',(-1.,0.,0.));
#14018=DIRECTION('center_axis',(1.,0.,0.));
#14019=DIRECTION('ref_axis',(0.,0.707106781186561,-0.707106781186534));
#14020=DIRECTION('center_axis',(-1.,0.,0.));
#14021=DIRECTION('ref_axis',(0.,1.,0.));
#14022=DIRECTION('',(-1.,0.,0.));
#14023=DIRECTION('',(1.,0.,0.));
#14024=DIRECTION('center_axis',(0.,0.,1.));
#14025=DIRECTION('ref_axis',(1.,0.,0.));
#14026=DIRECTION('center_axis',(0.,0.,-1.));
#14027=DIRECTION('ref_axis',(1.,0.,0.));
#14028=DIRECTION('center_axis',(0.,0.,1.));
#14029=DIRECTION('ref_axis',(1.,0.,0.));
#14030=DIRECTION('center_axis',(0.,0.,-1.));
#14031=DIRECTION('ref_axis',(0.,1.,0.));
#14032=DIRECTION('',(0.,0.,-1.));
#14033=DIRECTION('center_axis',(0.,0.,-1.));
#14034=DIRECTION('ref_axis',(-1.,0.,0.));
#14035=DIRECTION('',(0.,0.,-1.));
#14036=DIRECTION('center_axis',(0.,1.,0.));
#14037=DIRECTION('ref_axis',(1.,0.,0.));
#14038=DIRECTION('',(0.,0.,-1.));
#14039=DIRECTION('',(1.,0.,0.));
#14040=DIRECTION('center_axis',(0.,0.,-1.));
#14041=DIRECTION('ref_axis',(1.,0.,0.));
#14042=DIRECTION('',(-1.,0.,0.));
#14043=DIRECTION('',(0.,1.,0.));
#14044=DIRECTION('',(1.,0.,0.));
#14045=DIRECTION('',(0.,-1.,0.));
#14046=DIRECTION('center_axis',(0.,1.,0.));
#14047=DIRECTION('ref_axis',(0.,0.,-1.));
#14048=DIRECTION('center_axis',(-1.,0.,0.));
#14049=DIRECTION('ref_axis',(0.,0.,-1.));
#14050=DIRECTION('center_axis',(0.,1.,0.));
#14051=DIRECTION('ref_axis',(1.,0.,0.));
#14052=DIRECTION('center_axis',(0.,0.,-1.));
#14053=DIRECTION('ref_axis',(0.,-1.,0.));
#14054=DIRECTION('center_axis',(0.,-1.,0.));
#14055=DIRECTION('ref_axis',(0.70710678118654,0.,0.707106781186555));
#14056=DIRECTION('center_axis',(0.816496580927734,0.408248290463867,0.408248290463843));
#14057=DIRECTION('ref_axis',(0.577350269189598,-0.577350269189645,-0.577350269189634));
#14058=DIRECTION('center_axis',(1.,0.,0.));
#14059=DIRECTION('ref_axis',(0.,0.,-1.));
#14060=DIRECTION('center_axis',(0.,-1.,0.));
#14061=DIRECTION('ref_axis',(1.,0.,0.));
#14062=DIRECTION('center_axis',(9.25185853854317E-16,0.,-1.));
#14063=DIRECTION('ref_axis',(0.,-1.,0.));
#14064=DIRECTION('center_axis',(0.,1.,0.));
#14065=DIRECTION('ref_axis',(0.,0.,-1.));
#14066=DIRECTION('center_axis',(0.,1.,0.));
#14067=DIRECTION('ref_axis',(0.70710678118654,0.,0.707106781186555));
#14068=DIRECTION('center_axis',(0.,0.,-1.));
#14069=DIRECTION('ref_axis',(-1.,0.,0.));
#14070=DIRECTION('center_axis',(5.92118946466763E-14,-1.,0.));
#14071=DIRECTION('ref_axis',(0.,0.,1.));
#14072=DIRECTION('center_axis',(-1.,0.,0.));
#14073=DIRECTION('ref_axis',(0.,1.,0.));
#14074=DIRECTION('center_axis',(0.,0.,-1.));
#14075=DIRECTION('ref_axis',(-0.707106781186547,0.707106781186547,0.));
#14076=DIRECTION('',(0.,0.,1.));
#14077=DIRECTION('',(0.,0.,-1.));
#14078=DIRECTION('center_axis',(-0.707106781186576,0.,0.707106781186519));
#14079=DIRECTION('ref_axis',(0.707106781186519,0.,0.707106781186576));
#14080=DIRECTION('center_axis',(0.827465426020362,-0.538877990790925,-0.157833709270471));
#14081=DIRECTION('ref_axis',(-0.561516668266355,-0.794104487760816,-0.232587819494453));
#14082=DIRECTION('center_axis',(-0.707106781186544,3.663549070262E-14,-0.707106781186551));
#14083=DIRECTION('ref_axis',(-0.707106781186551,0.,0.707106781186544));
#14084=DIRECTION('center_axis',(0.,-1.,0.));
#14085=DIRECTION('ref_axis',(0.,0.,-1.));
#14086=DIRECTION('center_axis',(-1.,0.,-2.96059473233375E-14));
#14087=DIRECTION('ref_axis',(0.,-1.,0.));
#14088=DIRECTION('center_axis',(-0.408248290463871,-0.408248290463824,-0.816496580927742));
#14089=DIRECTION('ref_axis',(0.577350269189681,0.577350269189586,-0.57735026918961));
#14090=DIRECTION('center_axis',(0.,1.,0.));
#14091=DIRECTION('ref_axis',(0.,0.,-1.));
#14092=DIRECTION('center_axis',(1.,0.,5.9211894646675E-14));
#14093=DIRECTION('ref_axis',(0.,1.,0.));
#14094=DIRECTION('center_axis',(0.,9.25185853854317E-16,-1.));
#14095=DIRECTION('ref_axis',(1.,0.,0.));
#14096=DIRECTION('center_axis',(1.,0.,0.));
#14097=DIRECTION('ref_axis',(0.,0.707106781186519,-0.707106781186576));
#14098=DIRECTION('',(1.,0.,0.));
#14099=DIRECTION('',(-1.,0.,0.));
#14100=DIRECTION('center_axis',(0.408248290463859,-0.408248290463835,-0.816496580927742));
#14101=DIRECTION('ref_axis',(0.577350269189665,-0.577350269189618,0.577350269189594));
#14102=DIRECTION('center_axis',(0.,0.,1.));
#14103=DIRECTION('ref_axis',(1.,0.,0.));
#14104=DIRECTION('center_axis',(0.,-1.,0.));
#14105=DIRECTION('ref_axis',(0.,0.,1.));
#14106=DIRECTION('center_axis',(1.,0.,5.9211894646675E-14));
#14107=DIRECTION('ref_axis',(0.,-1.,0.));
#14108=DIRECTION('center_axis',(0.827465426020388,0.538877990790895,-0.157833709270442));
#14109=DIRECTION('ref_axis',(-0.561516668266318,0.794104487760845,-0.232587819494444));
#14110=DIRECTION('center_axis',(0.,1.,0.));
#14111=DIRECTION('ref_axis',(-0.707106781186544,0.,0.707106781186551));
#14112=DIRECTION('center_axis',(-0.70710678118657,0.,-0.707106781186525));
#14113=DIRECTION('ref_axis',(0.,1.,0.));
#14114=DIRECTION('center_axis',(-1.,-2.96059473233364E-14,0.));
#14115=DIRECTION('ref_axis',(0.,0.,-1.));
#14116=DIRECTION('center_axis',(-0.182143211721521,0.879465224064606,0.439732612032315));
#14117=DIRECTION('ref_axis',(-0.336556770590777,-0.475963149477983,0.812519920068737));
#14118=DIRECTION('center_axis',(-1.,0.,0.));
#14119=DIRECTION('ref_axis',(0.,0.,1.));
#14120=DIRECTION('center_axis',(0.,-1.,0.));
#14121=DIRECTION('ref_axis',(-0.707106781186551,0.,0.707106781186544));
#14122=DIRECTION('center_axis',(0.70710678118654,0.,0.707106781186555));
#14123=DIRECTION('ref_axis',(0.,-1.,0.));
#14124=DIRECTION('center_axis',(0.408248290463908,0.408248290463861,-0.816496580927704));
#14125=DIRECTION('ref_axis',(0.577350269189642,0.577350269189594,0.577350269189642));
#14126=DIRECTION('center_axis',(0.,1.,5.9211894646675E-14));
#14127=DIRECTION('ref_axis',(1.,0.,0.));
#14128=DIRECTION('center_axis',(0.,0.,1.));
#14129=DIRECTION('ref_axis',(0.,1.,0.));
#14130=DIRECTION('center_axis',(1.,0.,0.));
#14131=DIRECTION('ref_axis',(0.,0.,1.));
#14132=DIRECTION('center_axis',(0.,0.,1.));
#14133=DIRECTION('ref_axis',(0.707106781186589,0.707106781186506,0.));
#14134=DIRECTION('',(0.,0.,-1.));
#14135=DIRECTION('',(0.,0.,1.));
#14136=DIRECTION('center_axis',(0.182143211721517,0.879465224064606,-0.439732612032315));
#14137=DIRECTION('ref_axis',(-0.336556770590767,0.475963149477992,0.812519920068736));
#14138=DIRECTION('center_axis',(0.,1.,0.));
#14139=DIRECTION('ref_axis',(0.,0.,1.));
#14140=DIRECTION('center_axis',(-1.,0.,0.));
#14141=DIRECTION('ref_axis',(0.,1.,0.));
#14142=DIRECTION('center_axis',(0.70710678118654,0.,0.707106781186555));
#14143=DIRECTION('ref_axis',(-0.707106781186555,0.,0.70710678118654));
#14144=DIRECTION('center_axis',(1.,0.,0.));
#14145=DIRECTION('ref_axis',(0.,0.707106781186558,0.707106781186537));
#14146=DIRECTION('',(-1.,0.,0.));
#14147=DIRECTION('',(1.,0.,0.));
#14148=DIRECTION('center_axis',(0.707106781186547,0.,0.707106781186548));
#14149=DIRECTION('ref_axis',(-0.499999999999997,0.707106781186559,0.499999999999986));
#14150=DIRECTION('',(-0.707106781186547,0.,-0.707106781186548));
#14151=DIRECTION('',(0.707106781186547,0.,0.707106781186548));
#14152=DIRECTION('center_axis',(0.,-1.,0.));
#14153=DIRECTION('ref_axis',(-0.382683432365094,0.,0.923879532511285));
#14154=DIRECTION('',(0.,1.,0.));
#14155=DIRECTION('',(0.,-1.,0.));
#14156=DIRECTION('center_axis',(0.,-1.,0.));
#14157=DIRECTION('ref_axis',(0.707106781186558,0.,0.707106781186537));
#14158=DIRECTION('',(0.,1.,0.));
#14159=DIRECTION('',(0.,-1.,0.));
#14160=DIRECTION('center_axis',(-0.707106781186547,0.,-0.707106781186548));
#14161=DIRECTION('ref_axis',(-0.499999999999997,-0.707106781186559,0.499999999999986));
#14162=DIRECTION('',(0.707106781186547,0.,0.707106781186548));
#14163=DIRECTION('',(-0.707106781186547,0.,-0.707106781186548));
#14164=DIRECTION('center_axis',(-1.,0.,0.));
#14165=DIRECTION('ref_axis',(0.,-0.707106781186558,0.707106781186537));
#14166=DIRECTION('',(1.,0.,0.));
#14167=DIRECTION('',(-1.,0.,0.));
#14168=DIRECTION('center_axis',(-1.,0.,0.));
#14169=DIRECTION('ref_axis',(0.,0.707106781186561,-0.707106781186534));
#14170=DIRECTION('',(1.,0.,0.));
#14171=DIRECTION('center_axis',(0.,-1.,0.));
#14172=DIRECTION('ref_axis',(-0.923879532511297,0.,-0.382683432365066));
#14173=DIRECTION('',(0.,1.,0.));
#14174=DIRECTION('center_axis',(0.,0.,1.));
#14175=DIRECTION('ref_axis',(0.707106781186506,-0.707106781186589,0.));
#14176=DIRECTION('',(0.,0.,-1.));
#14177=DIRECTION('',(0.,0.,1.));
#14178=DIRECTION('center_axis',(0.,-1.,0.));
#14179=DIRECTION('ref_axis',(0.707106781186519,0.,-0.707106781186576));
#14180=DIRECTION('',(0.,1.,0.));
#14181=DIRECTION('',(0.,-1.,0.));
#14182=DIRECTION('center_axis',(1.,0.,0.));
#14183=DIRECTION('ref_axis',(0.,-0.707106781186561,-0.707106781186534));
#14184=DIRECTION('',(-1.,0.,0.));
#14185=DIRECTION('center_axis',(0.,-1.,0.));
#14186=DIRECTION('ref_axis',(0.707106781186519,0.,0.707106781186576));
#14187=DIRECTION('',(0.,-1.,0.));
#14188=DIRECTION('center_axis',(1.,0.,0.));
#14189=DIRECTION('ref_axis',(0.,-0.707106781186561,-0.707106781186534));
#14190=DIRECTION('',(1.,0.,0.));
#14191=DIRECTION('',(-1.,0.,0.));
#14192=DIRECTION('center_axis',(0.707106781186555,0.,-0.70710678118654));
#14193=DIRECTION('ref_axis',(-0.70710678118654,0.,-0.707106781186555));
#14194=DIRECTION('center_axis',(0.,0.,-1.));
#14195=DIRECTION('ref_axis',(-0.707106781186506,-0.707106781186589,0.));
#14196=DIRECTION('',(0.,0.,1.));
#14197=DIRECTION('',(0.,0.,-1.));
#14198=DIRECTION('center_axis',(-1.,0.,0.));
#14199=DIRECTION('ref_axis',(0.,0.,-1.));
#14200=DIRECTION('',(0.,-1.,0.));
#14201=DIRECTION('center_axis',(0.,-1.,0.));
#14202=DIRECTION('ref_axis',(-1.,0.,0.));
#14203=DIRECTION('center_axis',(1.,0.,0.));
#14204=DIRECTION('ref_axis',(0.,0.,1.));
#14205=DIRECTION('center_axis',(0.,0.,1.));
#14206=DIRECTION('ref_axis',(-1.,0.,0.));
#14207=DIRECTION('',(-1.,0.,0.));
#14208=DIRECTION('center_axis',(0.,0.,1.));
#14209=DIRECTION('ref_axis',(1.,0.,0.));
#14210=DIRECTION('',(1.,0.,0.));
#14211=DIRECTION('center_axis',(0.,0.,1.));
#14212=DIRECTION('ref_axis',(-1.,0.,0.));
#14213=DIRECTION('center_axis',(-0.707106781186548,0.,0.707106781186547));
#14214=DIRECTION('ref_axis',(-0.707106781186547,0.,-0.707106781186548));
#14215=DIRECTION('center_axis',(0.,-1.,0.));
#14216=DIRECTION('ref_axis',(0.,0.,1.));
#14217=DIRECTION('center_axis',(1.,0.,0.));
#14218=DIRECTION('ref_axis',(0.,-0.707106781186516,0.707106781186579));
#14219=DIRECTION('center_axis',(1.,0.,0.));
#14220=DIRECTION('ref_axis',(0.,0.,1.));
#14221=DIRECTION('center_axis',(-1.,0.,0.));
#14222=DIRECTION('ref_axis',(0.,-1.,0.));
#14223=DIRECTION('center_axis',(0.,0.,-1.));
#14224=DIRECTION('ref_axis',(1.,0.,0.));
#14225=DIRECTION('center_axis',(1.,0.,0.));
#14226=DIRECTION('ref_axis',(0.,1.,0.));
#14227=DIRECTION('center_axis',(0.,0.,-1.));
#14228=DIRECTION('ref_axis',(1.,0.,0.));
#14229=DIRECTION('center_axis',(-1.,0.,0.));
#14230=DIRECTION('ref_axis',(0.,0.707106781186558,0.707106781186537));
#14231=DIRECTION('center_axis',(1.,0.,0.));
#14232=DIRECTION('ref_axis',(0.,1.,0.));
#14233=DIRECTION('',(-1.,0.,0.));
#14234=DIRECTION('center_axis',(0.,0.,-1.));
#14235=DIRECTION('ref_axis',(-1.,0.,0.));
#14236=DIRECTION('center_axis',(0.,0.,-1.));
#14237=DIRECTION('ref_axis',(0.,-1.,0.));
#14238=DIRECTION('',(0.,0.,-1.));
#14239=DIRECTION('center_axis',(0.,-1.,0.));
#14240=DIRECTION('ref_axis',(-1.,0.,0.));
#14241=DIRECTION('center_axis',(0.,0.,-1.));
#14242=DIRECTION('ref_axis',(1.,0.,0.));
#14243=DIRECTION('',(0.,0.,1.));
#14244=DIRECTION('',(1.,0.,0.));
#14245=DIRECTION('',(0.,0.,1.));
#14246=DIRECTION('',(1.,0.,0.));
#14247=DIRECTION('',(0.,0.,1.));
#14248=DIRECTION('',(1.,0.,0.));
#14249=DIRECTION('',(0.,0.,1.));
#14250=DIRECTION('',(1.,0.,0.));
#14251=DIRECTION('',(0.,0.,1.));
#14252=DIRECTION('',(1.,0.,0.));
#14253=DIRECTION('',(0.,0.,1.));
#14254=DIRECTION('',(1.,0.,0.));
#14255=DIRECTION('',(0.,0.,1.));
#14256=DIRECTION('',(1.,0.,0.));
#14257=DIRECTION('',(0.,0.,1.));
#14258=DIRECTION('',(1.,0.,0.));
#14259=DIRECTION('',(0.,0.,1.));
#14260=DIRECTION('',(1.,0.,0.));
#14261=DIRECTION('',(0.,0.,1.));
#14262=DIRECTION('',(1.,0.,0.));
#14263=CARTESIAN_POINT('',(0.,0.,0.));
#14264=CARTESIAN_POINT('',(0.,0.,0.));
#14265=CARTESIAN_POINT('Origin',(0.,-115.,16.0775024873567));
#14266=CARTESIAN_POINT('',(-8.,-115.,16.0775024873567));
#14267=CARTESIAN_POINT('Origin',(0.,-115.,16.0775024873567));
#14268=CARTESIAN_POINT('',(-7.5,-115.,16.0775024873567));
#14269=CARTESIAN_POINT('Origin',(0.,-115.,16.0775024873567));
#14270=CARTESIAN_POINT('Origin',(0.,-134.5,16.0775024873567));
#14271=CARTESIAN_POINT('',(-8.,-135.,16.0775024873567));
#14272=CARTESIAN_POINT('Origin',(0.,-135.,16.0775024873567));
#14273=CARTESIAN_POINT('',(-9.,-134.,16.0775024873567));
#14274=CARTESIAN_POINT('',(-8.5,-134.5,16.0775024873567));
#14275=CARTESIAN_POINT('Origin',(0.,-134.,16.0775024873567));
#14276=CARTESIAN_POINT('Origin',(0.,-115.,16.0775024873567));
#14277=CARTESIAN_POINT('',(-9.,-116.,16.0775024873567));
#14278=CARTESIAN_POINT('',(-9.,-115.,16.0775024873567));
#14279=CARTESIAN_POINT('Origin',(0.,-116.,16.0775024873567));
#14280=CARTESIAN_POINT('Origin',(0.,-135.,16.0775024873567));
#14281=CARTESIAN_POINT('Origin',(0.,-115.5,16.0775024873567));
#14282=CARTESIAN_POINT('',(-8.5,-115.5,16.0775024873567));
#14283=CARTESIAN_POINT('Origin',(0.,-90.,16.0775024873567));
#14284=CARTESIAN_POINT('',(-7.5,-90.,16.0775024873567));
#14285=CARTESIAN_POINT('',(-7.5,-90.,16.0775024873567));
#14286=CARTESIAN_POINT('Origin',(0.,-90.,16.0775024873567));
#14287=CARTESIAN_POINT('Origin',(0.,-90.,16.0775024873567));
#14288=CARTESIAN_POINT('',(0.,0.,0.));
#14289=CARTESIAN_POINT('Origin',(65.,0.,6.28953555269655));
#14290=CARTESIAN_POINT('',(64.5,-90.,6.28953555269655));
#14291=CARTESIAN_POINT('',(65.,-89.5,6.28953555269655));
#14292=CARTESIAN_POINT('Origin',(64.5,-89.5,6.28953555269655));
#14293=CARTESIAN_POINT('',(62.,-90.,6.28953555269655));
#14294=CARTESIAN_POINT('',(0.,-90.,6.28953555269655));
#14295=CARTESIAN_POINT('',(62.,90.,6.28953555269655));
#14296=CARTESIAN_POINT('',(62.,0.,6.28953555269655));
#14297=CARTESIAN_POINT('',(64.5,90.,6.28953555269655));
#14298=CARTESIAN_POINT('',(65.,90.,6.28953555269655));
#14299=CARTESIAN_POINT('',(65.,89.5,6.28953555269655));
#14300=CARTESIAN_POINT('Origin',(64.5,89.5,6.28953555269655));
#14301=CARTESIAN_POINT('',(65.,-45.,6.28953555269655));
#14302=CARTESIAN_POINT('Origin',(62.,0.,2.78953555269655));
#14303=CARTESIAN_POINT('',(65.,-89.5,2.78953555269655));
#14304=CARTESIAN_POINT('',(64.5,-90.,2.78953555269655));
#14305=CARTESIAN_POINT('Origin',(64.5,-89.5,2.78953555269655));
#14306=CARTESIAN_POINT('',(65.,89.5,2.78953555269655));
#14307=CARTESIAN_POINT('',(65.,-45.,2.78953555269655));
#14308=CARTESIAN_POINT('',(64.5,90.,2.78953555269655));
#14309=CARTESIAN_POINT('Origin',(64.5,89.5,2.78953555269655));
#14310=CARTESIAN_POINT('',(62.,90.,2.78953555269655));
#14311=CARTESIAN_POINT('',(63.5,90.,2.78953555269655));
#14312=CARTESIAN_POINT('',(62.,-90.,2.78953555269655));
#14313=CARTESIAN_POINT('',(62.,0.,2.78953555269655));
#14314=CARTESIAN_POINT('',(-1.5,-90.,2.78953555269655));
#14315=CARTESIAN_POINT('Origin',(62.,0.,6.28953555269655));
#14316=CARTESIAN_POINT('',(62.,90.,3.14476777634828));
#14317=CARTESIAN_POINT('',(62.,-90.,3.14476777634828));
#14318=CARTESIAN_POINT('Origin',(64.5,-89.5,0.));
#14319=CARTESIAN_POINT('',(64.5,-90.,0.5));
#14320=CARTESIAN_POINT('',(64.5,-90.,0.));
#14321=CARTESIAN_POINT('',(65.,-89.5,0.));
#14322=CARTESIAN_POINT('Origin',(64.5,-89.5,0.5));
#14323=CARTESIAN_POINT('',(65.,-89.5,0.));
#14324=CARTESIAN_POINT('Origin',(64.5,-89.5,0.));
#14325=CARTESIAN_POINT('',(65.,-89.5,19.5));
#14326=CARTESIAN_POINT('',(65.,-89.5,0.));
#14327=CARTESIAN_POINT('',(64.5,-90.,19.5));
#14328=CARTESIAN_POINT('Origin',(64.5,-89.5,19.5));
#14329=CARTESIAN_POINT('',(64.5,-90.,0.));
#14330=CARTESIAN_POINT('Origin',(65.,-90.,0.));
#14331=CARTESIAN_POINT('',(65.,89.5,0.));
#14332=CARTESIAN_POINT('',(65.,-90.,0.));
#14333=CARTESIAN_POINT('',(65.,89.5,0.));
#14334=CARTESIAN_POINT('Origin',(65.,-90.,0.));
#14335=CARTESIAN_POINT('',(65.,89.5,19.5));
#14336=CARTESIAN_POINT('',(65.,89.5,0.));
#14337=CARTESIAN_POINT('',(65.,-45.,19.5));
#14338=CARTESIAN_POINT('Origin',(64.5,89.5,0.));
#14339=CARTESIAN_POINT('',(64.5,90.,0.5));
#14340=CARTESIAN_POINT('Origin',(64.5,89.5,0.5));
#14341=CARTESIAN_POINT('',(64.5,90.,0.));
#14342=CARTESIAN_POINT('Origin',(64.5,89.5,0.));
#14343=CARTESIAN_POINT('',(64.5,90.,19.5));
#14344=CARTESIAN_POINT('',(64.5,90.,0.));
#14345=CARTESIAN_POINT('Origin',(64.5,89.5,19.5));
#14346=CARTESIAN_POINT('Origin',(65.,90.,0.));
#14347=CARTESIAN_POINT('',(-64.5,90.,0.5));
#14348=CARTESIAN_POINT('',(32.5,90.,0.5));
#14349=CARTESIAN_POINT('',(-64.5,90.,2.78953555269655));
#14350=CARTESIAN_POINT('',(-64.5,90.,0.));
#14351=CARTESIAN_POINT('',(-62.,90.,2.78953555269655));
#14352=CARTESIAN_POINT('',(1.5,90.,2.78953555269655));
#14353=CARTESIAN_POINT('',(-62.,90.,6.28953555269655));
#14354=CARTESIAN_POINT('',(-62.,90.,3.14476777634828));
#14355=CARTESIAN_POINT('',(-64.5,90.,6.28953555269655));
#14356=CARTESIAN_POINT('',(0.,90.,6.28953555269655));
#14357=CARTESIAN_POINT('',(-64.5,90.,19.5));
#14358=CARTESIAN_POINT('',(-64.5,90.,0.));
#14359=CARTESIAN_POINT('',(-23.0395928638606,90.,19.5));
#14360=CARTESIAN_POINT('',(32.5,90.,19.5));
#14361=CARTESIAN_POINT('',(-25.6346603396366,90.,16.904932524224));
#14362=CARTESIAN_POINT('',(-5.47791795259883,90.,37.0616749112618));
#14363=CARTESIAN_POINT('',(-24.92755355845,90.,15.1978257430375));
#14364=CARTESIAN_POINT('Origin',(-24.92755355845,90.,16.1978257430375));
#14365=CARTESIAN_POINT('',(-19.5453000725091,90.,15.1978257430375));
#14366=CARTESIAN_POINT('',(19.4326698301817,90.,15.1978257430375));
#14367=CARTESIAN_POINT('',(-19.5453000725091,90.,4.19782574303749));
#14368=CARTESIAN_POINT('',(-19.5453000725091,90.,7.84891287151875));
#14369=CARTESIAN_POINT('',(-18.545300072509,90.,3.19782574303749));
#14370=CARTESIAN_POINT('Origin',(-18.545300072509,90.,4.19782574303749));
#14371=CARTESIAN_POINT('',(21.0741207385024,90.,3.19782574303749));
#14372=CARTESIAN_POINT('',(22.9773499637455,90.,3.19782574303749));
#14373=CARTESIAN_POINT('',(22.0741207385024,90.,4.19782574303749));
#14374=CARTESIAN_POINT('Origin',(21.0741207385024,90.,4.19782574303749));
#14375=CARTESIAN_POINT('',(22.0741207385024,90.,15.1978257430375));
#14376=CARTESIAN_POINT('',(22.0741207385024,90.,1.84891287151875));
#14377=CARTESIAN_POINT('',(44.3272645584125,90.,15.1978257430375));
#14378=CARTESIAN_POINT('',(43.2870603692512,90.,15.1978257430375));
#14379=CARTESIAN_POINT('',(45.3272645584125,90.,16.1978257430375));
#14380=CARTESIAN_POINT('Origin',(44.3272645584125,90.,16.1978257430375));
#14381=CARTESIAN_POINT('',(45.3272645584125,90.,19.5));
#14382=CARTESIAN_POINT('',(45.3272645584125,90.,7.84891287151875));
#14383=CARTESIAN_POINT('',(32.5,90.,19.5));
#14384=CARTESIAN_POINT('Origin',(-65.,0.,6.28953555269655));
#14385=CARTESIAN_POINT('',(-65.,89.5,6.28953555269655));
#14386=CARTESIAN_POINT('Origin',(-64.5,89.5,6.28953555269655));
#14387=CARTESIAN_POINT('',(-62.,-90.,6.28953555269655));
#14388=CARTESIAN_POINT('',(-62.,0.,6.28953555269655));
#14389=CARTESIAN_POINT('',(-64.5,-90.,6.28953555269655));
#14390=CARTESIAN_POINT('',(-65.,-90.,6.28953555269655));
#14391=CARTESIAN_POINT('',(-65.,-89.5,6.28953555269655));
#14392=CARTESIAN_POINT('Origin',(-64.5,-89.5,6.28953555269655));
#14393=CARTESIAN_POINT('',(-65.,45.,6.28953555269655));
#14394=CARTESIAN_POINT('Origin',(-62.,0.,2.78953555269655));
#14395=CARTESIAN_POINT('',(-65.,89.5,2.78953555269655));
#14396=CARTESIAN_POINT('Origin',(-64.5,89.5,2.78953555269655));
#14397=CARTESIAN_POINT('',(-65.,-89.5,2.78953555269655));
#14398=CARTESIAN_POINT('',(-65.,45.,2.78953555269655));
#14399=CARTESIAN_POINT('',(-64.5,-90.,2.78953555269655));
#14400=CARTESIAN_POINT('Origin',(-64.5,-89.5,2.78953555269655));
#14401=CARTESIAN_POINT('',(-62.,-90.,2.78953555269655));
#14402=CARTESIAN_POINT('',(-63.5,-90.,2.78953555269655));
#14403=CARTESIAN_POINT('',(-62.,0.,2.78953555269655));
#14404=CARTESIAN_POINT('Origin',(-62.,0.,6.28953555269655));
#14405=CARTESIAN_POINT('',(-62.,-90.,3.14476777634828));
#14406=CARTESIAN_POINT('Origin',(-64.5,89.5,0.));
#14407=CARTESIAN_POINT('',(-65.,89.5,19.5));
#14408=CARTESIAN_POINT('',(-65.,89.5,0.));
#14409=CARTESIAN_POINT('Origin',(-64.5,89.5,19.5));
#14410=CARTESIAN_POINT('Origin',(-65.,-90.,0.));
#14411=CARTESIAN_POINT('',(45.3272645584125,-90.,19.5));
#14412=CARTESIAN_POINT('',(-32.5,-90.,19.5));
#14413=CARTESIAN_POINT('',(45.3272645584125,-90.,16.1978257430375));
#14414=CARTESIAN_POINT('',(45.3272645584125,-90.,7.84891287151875));
#14415=CARTESIAN_POINT('',(44.3272645584124,-90.,15.1978257430375));
#14416=CARTESIAN_POINT('Origin',(44.3272645584124,-90.,16.1978257430375));
#14417=CARTESIAN_POINT('',(22.0741207385024,-90.,15.1978257430375));
#14418=CARTESIAN_POINT('',(-21.7129396307488,-90.,15.1978257430375));
#14419=CARTESIAN_POINT('',(22.0741207385024,-90.,4.19782574303749));
#14420=CARTESIAN_POINT('',(22.0741207385024,-90.,1.84891287151875));
#14421=CARTESIAN_POINT('',(21.0741207385024,-90.,3.19782574303749));
#14422=CARTESIAN_POINT('Origin',(21.0741207385024,-90.,4.19782574303749));
#14423=CARTESIAN_POINT('',(-18.545300072509,-90.,3.19782574303749));
#14424=CARTESIAN_POINT('',(-42.0226500362545,-90.,3.19782574303749));
#14425=CARTESIAN_POINT('',(-19.545300072509,-90.,4.19782574303749));
#14426=CARTESIAN_POINT('Origin',(-18.545300072509,-90.,4.19782574303749));
#14427=CARTESIAN_POINT('',(-19.545300072509,-90.,15.1978257430375));
#14428=CARTESIAN_POINT('',(-19.545300072509,-90.,7.84891287151875));
#14429=CARTESIAN_POINT('',(-24.92755355845,-90.,15.1978257430375));
#14430=CARTESIAN_POINT('',(-45.5673301698183,-90.,15.1978257430375));
#14431=CARTESIAN_POINT('',(-25.6346603396366,-90.,16.904932524224));
#14432=CARTESIAN_POINT('Origin',(-24.92755355845,-90.,16.1978257430375));
#14433=CARTESIAN_POINT('',(-23.0395928638606,-90.,19.5));
#14434=CARTESIAN_POINT('',(-37.9779179525988,-90.,4.56167491126179));
#14435=CARTESIAN_POINT('',(-64.5,-90.,19.5));
#14436=CARTESIAN_POINT('',(-32.5,-90.,19.5));
#14437=CARTESIAN_POINT('',(-64.5,-90.,0.));
#14438=CARTESIAN_POINT('',(-64.5,-90.,0.5));
#14439=CARTESIAN_POINT('',(-64.5,-90.,0.));
#14440=CARTESIAN_POINT('',(-32.5,-90.,0.5));
#14441=CARTESIAN_POINT('Origin',(-65.,90.,0.));
#14442=CARTESIAN_POINT('',(-65.,-89.5,19.5));
#14443=CARTESIAN_POINT('',(-65.,-89.5,0.));
#14444=CARTESIAN_POINT('',(-65.,45.,19.5));
#14445=CARTESIAN_POINT('Origin',(-64.5,-89.5,0.));
#14446=CARTESIAN_POINT('',(-65.,-89.5,0.5));
#14447=CARTESIAN_POINT('',(-65.,-89.5,0.));
#14448=CARTESIAN_POINT('Origin',(-64.5,-89.5,0.5));
#14449=CARTESIAN_POINT('Origin',(44.3272645584125,89.5,16.1978257430375));
#14450=CARTESIAN_POINT('',(44.3272645584125,89.5,15.6978257430375));
#14451=CARTESIAN_POINT('Origin',(44.3272645584125,89.5,15.1978257430375));
#14452=CARTESIAN_POINT('',(44.8272645584125,89.5,16.1978257430375));
#14453=CARTESIAN_POINT('Origin',(44.3272645584125,89.5,16.1978257430375));
#14454=CARTESIAN_POINT('Origin',(45.3272645584125,89.5,16.1978257430375));
#14455=CARTESIAN_POINT('Origin',(44.3272645584124,-89.5,16.1978257430375));
#14456=CARTESIAN_POINT('',(44.8272645584125,-89.5,16.1978257430375));
#14457=CARTESIAN_POINT('Origin',(45.3272645584125,-89.5,16.1978257430375));
#14458=CARTESIAN_POINT('',(44.3272645584124,-89.5,15.6978257430375));
#14459=CARTESIAN_POINT('Origin',(44.3272645584125,-89.5,16.1978257430375));
#14460=CARTESIAN_POINT('Origin',(44.3272645584124,-89.5,15.1978257430375));
#14461=CARTESIAN_POINT('Origin',(22.0741207385024,89.5,15.1978257430375));
#14462=CARTESIAN_POINT('',(22.0741207385024,89.5,15.6978257430375));
#14463=CARTESIAN_POINT('Origin',(22.0741207385024,89.5,15.1978257430375));
#14464=CARTESIAN_POINT('',(21.5741207385024,89.5,15.1978257430375));
#14465=CARTESIAN_POINT('Origin',(22.0741207385024,89.5,15.1978257430375));
#14466=CARTESIAN_POINT('Origin',(22.0741207385024,89.5,15.1978257430375));
#14467=CARTESIAN_POINT('Origin',(45.3272645584125,89.5,19.5));
#14468=CARTESIAN_POINT('',(45.3272645584125,89.5,20.));
#14469=CARTESIAN_POINT('Origin',(45.3272645584125,89.5,19.5));
#14470=CARTESIAN_POINT('',(44.8272645584125,89.5,19.5));
#14471=CARTESIAN_POINT('Origin',(45.3272645584125,89.5,19.5));
#14472=CARTESIAN_POINT('Origin',(45.3272645584125,89.5,19.5));
#14473=CARTESIAN_POINT('Origin',(45.3272645584125,89.5,7.84891287151875));
#14474=CARTESIAN_POINT('',(44.8272645584125,89.5,7.84891287151875));
#14475=CARTESIAN_POINT('Origin',(22.0741207385024,-89.5,15.1978257430375));
#14476=CARTESIAN_POINT('',(21.5741207385024,-89.5,15.1978257430375));
#14477=CARTESIAN_POINT('Origin',(22.0741207385024,-89.5,15.1978257430375));
#14478=CARTESIAN_POINT('',(22.0741207385024,-89.5,15.6978257430375));
#14479=CARTESIAN_POINT('Origin',(22.0741207385024,-89.5,15.1978257430375));
#14480=CARTESIAN_POINT('Origin',(22.0741207385024,-89.5,15.1978257430375));
#14481=CARTESIAN_POINT('Origin',(-21.7129396307488,-89.5,15.1978257430375));
#14482=CARTESIAN_POINT('',(-21.7129396307488,-89.5,15.6978257430375));
#14483=CARTESIAN_POINT('Origin',(22.0741207385024,-90.,15.1978257430375));
#14484=CARTESIAN_POINT('',(22.0741207385024,-90.,15.6978257430375));
#14485=CARTESIAN_POINT('',(21.5741207385024,-90.,15.1978257430375));
#14486=CARTESIAN_POINT('Origin',(45.3272645584125,-89.5,19.5));
#14487=CARTESIAN_POINT('',(45.3272645584125,-89.5,20.));
#14488=CARTESIAN_POINT('Origin',(45.3272645584125,-89.5,19.5));
#14489=CARTESIAN_POINT('',(44.8272645584125,-89.5,19.5));
#14490=CARTESIAN_POINT('Origin',(45.3272645584125,-89.5,19.5));
#14491=CARTESIAN_POINT('Origin',(45.3272645584125,-89.5,19.5));
#14492=CARTESIAN_POINT('Origin',(45.3272645584125,-45.,19.5));
#14493=CARTESIAN_POINT('',(45.3272645584125,-45.,20.));
#14494=CARTESIAN_POINT('',(44.8272645584125,-45.,19.5));
#14495=CARTESIAN_POINT('Origin',(45.3272645584125,-89.5,7.84891287151875));
#14496=CARTESIAN_POINT('',(44.8272645584125,-89.5,7.84891287151875));
#14497=CARTESIAN_POINT('Origin',(21.0741207385024,89.5,4.19782574303749));
#14498=CARTESIAN_POINT('',(21.0741207385024,89.5,3.69782574303749));
#14499=CARTESIAN_POINT('Origin',(21.0741207385024,89.5,3.19782574303749));
#14500=CARTESIAN_POINT('',(21.5741207385024,89.5,4.19782574303749));
#14501=CARTESIAN_POINT('Origin',(21.0741207385024,89.5,4.19782574303749));
#14502=CARTESIAN_POINT('Origin',(22.0741207385024,89.5,4.19782574303749));
#14503=CARTESIAN_POINT('Origin',(64.5,89.5,19.5));
#14504=CARTESIAN_POINT('',(64.5,89.5,20.));
#14505=CARTESIAN_POINT('Origin',(64.5,89.5,19.5));
#14506=CARTESIAN_POINT('Origin',(64.5,89.5,19.5));
#14507=CARTESIAN_POINT('Origin',(21.0741207385024,-89.5,4.19782574303749));
#14508=CARTESIAN_POINT('',(21.5741207385024,-89.5,4.19782574303749));
#14509=CARTESIAN_POINT('Origin',(22.0741207385024,-89.5,4.19782574303749));
#14510=CARTESIAN_POINT('',(21.0741207385024,-89.5,3.69782574303749));
#14511=CARTESIAN_POINT('Origin',(21.0741207385024,-89.5,4.19782574303749));
#14512=CARTESIAN_POINT('Origin',(21.0741207385024,-89.5,3.19782574303749));
#14513=CARTESIAN_POINT('Origin',(22.0741207385024,-89.5,1.84891287151875));
#14514=CARTESIAN_POINT('',(21.5741207385024,-89.5,1.84891287151875));
#14515=CARTESIAN_POINT('Origin',(21.0741207385024,-90.,4.19782574303749));
#14516=CARTESIAN_POINT('',(21.5741207385024,-90.,4.19782574303749));
#14517=CARTESIAN_POINT('',(21.0741207385024,-90.,3.69782574303749));
#14518=CARTESIAN_POINT('Origin',(64.5,-89.5,19.5));
#14519=CARTESIAN_POINT('',(64.5,-89.5,20.));
#14520=CARTESIAN_POINT('Origin',(64.5,-89.5,19.5));
#14521=CARTESIAN_POINT('Origin',(64.5,-89.5,19.5));
#14522=CARTESIAN_POINT('Origin',(-18.545300072509,89.5,4.19782574303749));
#14523=CARTESIAN_POINT('',(-19.045300072509,89.5,4.19782574303749));
#14524=CARTESIAN_POINT('Origin',(-19.5453000725091,89.5,4.19782574303749));
#14525=CARTESIAN_POINT('',(-18.545300072509,89.5,3.69782574303749));
#14526=CARTESIAN_POINT('Origin',(-18.545300072509,89.5,4.19782574303749));
#14527=CARTESIAN_POINT('Origin',(-18.545300072509,89.5,3.19782574303749));
#14528=CARTESIAN_POINT('Origin',(-18.545300072509,-89.5,4.19782574303749));
#14529=CARTESIAN_POINT('',(-18.545300072509,-89.5,3.69782574303749));
#14530=CARTESIAN_POINT('Origin',(-18.545300072509,-89.5,3.19782574303749));
#14531=CARTESIAN_POINT('',(-19.045300072509,-89.5,4.19782574303749));
#14532=CARTESIAN_POINT('Origin',(-18.545300072509,-89.5,4.19782574303749));
#14533=CARTESIAN_POINT('Origin',(-19.545300072509,-89.5,4.19782574303749));
#14534=CARTESIAN_POINT('Origin',(-42.0226500362545,-89.5,3.19782574303749));
#14535=CARTESIAN_POINT('',(-42.0226500362545,-89.5,3.69782574303749));
#14536=CARTESIAN_POINT('Origin',(-18.545300072509,-90.,4.19782574303749));
#14537=CARTESIAN_POINT('',(-18.545300072509,-90.,3.69782574303749));
#14538=CARTESIAN_POINT('',(-19.045300072509,-90.,4.19782574303749));
#14539=CARTESIAN_POINT('Origin',(-19.545300072509,89.5,15.1978257430375));
#14540=CARTESIAN_POINT('',(-19.045300072509,89.5,15.1978257430375));
#14541=CARTESIAN_POINT('Origin',(-19.5453000725091,89.5,15.1978257430375));
#14542=CARTESIAN_POINT('',(-19.545300072509,89.5,15.6978257430375));
#14543=CARTESIAN_POINT('Origin',(-19.545300072509,89.5,15.1978257430375));
#14544=CARTESIAN_POINT('Origin',(-19.545300072509,89.5,15.1978257430375));
#14545=CARTESIAN_POINT('Origin',(-64.5,89.5,0.5));
#14546=CARTESIAN_POINT('',(-65.,89.5,0.5));
#14547=CARTESIAN_POINT('Origin',(-64.5,89.5,0.5));
#14548=CARTESIAN_POINT('',(-64.5,89.5,0.));
#14549=CARTESIAN_POINT('Origin',(-64.5,89.5,0.5));
#14550=CARTESIAN_POINT('Origin',(-64.5,89.5,0.5));
#14551=CARTESIAN_POINT('Origin',(32.5,89.5,0.5));
#14552=CARTESIAN_POINT('',(32.5,89.5,0.));
#14553=CARTESIAN_POINT('Origin',(-19.545300072509,-89.5,15.1978257430375));
#14554=CARTESIAN_POINT('',(-19.545300072509,-89.5,15.6978257430375));
#14555=CARTESIAN_POINT('Origin',(-19.545300072509,-89.5,15.1978257430375));
#14556=CARTESIAN_POINT('',(-19.045300072509,-89.5,15.1978257430375));
#14557=CARTESIAN_POINT('Origin',(-19.545300072509,-89.5,15.1978257430375));
#14558=CARTESIAN_POINT('Origin',(-19.545300072509,-89.5,15.1978257430375));
#14559=CARTESIAN_POINT('Origin',(-19.545300072509,-89.5,7.84891287151875));
#14560=CARTESIAN_POINT('',(-19.045300072509,-89.5,7.84891287151875));
#14561=CARTESIAN_POINT('Origin',(-19.545300072509,-90.,15.1978257430375));
#14562=CARTESIAN_POINT('',(-19.045300072509,-90.,15.1978257430375));
#14563=CARTESIAN_POINT('',(-19.545300072509,-90.,15.6978257430375));
#14564=CARTESIAN_POINT('Origin',(-64.5,-89.5,0.5));
#14565=CARTESIAN_POINT('',(-64.5,-89.5,0.));
#14566=CARTESIAN_POINT('Origin',(-64.5,-89.5,0.5));
#14567=CARTESIAN_POINT('Origin',(-64.5,-89.5,0.5));
#14568=CARTESIAN_POINT('Origin',(-64.5,45.,0.5));
#14569=CARTESIAN_POINT('',(-65.,45.,0.5));
#14570=CARTESIAN_POINT('',(-64.5,45.,0.));
#14571=CARTESIAN_POINT('Origin',(-32.5,-89.5,0.5));
#14572=CARTESIAN_POINT('',(-32.5,-89.5,0.));
#14573=CARTESIAN_POINT('Origin',(-24.92755355845,89.5,16.1978257430375));
#14574=CARTESIAN_POINT('',(-25.2811069490433,89.5,16.5513791336308));
#14575=CARTESIAN_POINT('Origin',(-25.6346603396366,89.5,16.904932524224));
#14576=CARTESIAN_POINT('',(-24.92755355845,89.5,15.6978257430375));
#14577=CARTESIAN_POINT('Origin',(-24.92755355845,89.5,16.1978257430375));
#14578=CARTESIAN_POINT('Origin',(-24.92755355845,89.5,15.1978257430375));
#14579=CARTESIAN_POINT('Origin',(-64.5,89.5,19.5));
#14580=CARTESIAN_POINT('',(-64.5,89.5,20.));
#14581=CARTESIAN_POINT('Origin',(-64.5,89.5,19.5));
#14582=CARTESIAN_POINT('Origin',(-64.5,89.5,19.5));
#14583=CARTESIAN_POINT('Origin',(-64.5,89.5,0.));
#14584=CARTESIAN_POINT('',(-65.,89.5,0.));
#14585=CARTESIAN_POINT('Origin',(-24.92755355845,-89.5,16.1978257430375));
#14586=CARTESIAN_POINT('',(-24.92755355845,-89.5,15.6978257430375));
#14587=CARTESIAN_POINT('Origin',(-24.92755355845,-89.5,15.1978257430375));
#14588=CARTESIAN_POINT('',(-25.2811069490433,-89.5,16.5513791336308));
#14589=CARTESIAN_POINT('Origin',(-24.92755355845,-89.5,16.1978257430375));
#14590=CARTESIAN_POINT('Origin',(-25.6346603396366,-89.5,16.904932524224));
#14591=CARTESIAN_POINT('Origin',(-64.5,-89.5,19.5));
#14592=CARTESIAN_POINT('',(-64.5,-89.5,20.));
#14593=CARTESIAN_POINT('Origin',(-64.5,-89.5,19.5));
#14594=CARTESIAN_POINT('Origin',(-64.5,-89.5,19.5));
#14595=CARTESIAN_POINT('Origin',(-64.5,-89.5,19.5));
#14596=CARTESIAN_POINT('Origin',(-64.5,-89.5,0.));
#14597=CARTESIAN_POINT('Origin',(-23.0395928638606,89.5,19.5));
#14598=CARTESIAN_POINT('',(-22.6860394732673,89.5,19.1464466094067));
#14599=CARTESIAN_POINT('',(-23.0395928638606,89.5,20.));
#14600=CARTESIAN_POINT('Origin',(-23.0395928638606,89.5,19.5));
#14601=CARTESIAN_POINT('Origin',(-23.0395928638606,89.5,19.5));
#14602=CARTESIAN_POINT('Origin',(-23.0395928638606,89.5,19.5));
#14603=CARTESIAN_POINT('Origin',(-5.47791795259883,89.5,37.0616749112618));
#14604=CARTESIAN_POINT('',(-5.12436456200555,89.5,36.7081215206685));
#14605=CARTESIAN_POINT('Origin',(32.5,89.5,19.5));
#14606=CARTESIAN_POINT('',(32.5,89.5,20.));
#14607=CARTESIAN_POINT('Origin',(-23.0395928638606,-89.5,19.5));
#14608=CARTESIAN_POINT('',(-22.6860394732673,-89.5,19.1464466094067));
#14609=CARTESIAN_POINT('Origin',(-23.0395928638606,-89.5,19.5));
#14610=CARTESIAN_POINT('',(-23.0395928638606,-89.5,20.));
#14611=CARTESIAN_POINT('Origin',(-23.0395928638606,-89.5,19.5));
#14612=CARTESIAN_POINT('Origin',(-23.0395928638606,-89.5,19.5));
#14613=CARTESIAN_POINT('Origin',(-23.0395928638606,-45.,19.5));
#14614=CARTESIAN_POINT('',(-23.0395928638606,-45.,20.));
#14615=CARTESIAN_POINT('',(-22.6860394732673,-45.,19.1464466094067));
#14616=CARTESIAN_POINT('Origin',(-32.5,-89.5,19.5));
#14617=CARTESIAN_POINT('',(-32.5,-89.5,20.));
#14618=CARTESIAN_POINT('Origin',(-37.9779179525988,-89.5,4.56167491126179));
#14619=CARTESIAN_POINT('',(-37.6243645620056,-89.5,4.20812152066852));
#14620=CARTESIAN_POINT('Origin',(-64.5,45.,19.5));
#14621=CARTESIAN_POINT('',(-64.5,45.,20.));
#14622=CARTESIAN_POINT('Origin',(-45.5673301698183,-89.5,15.1978257430375));
#14623=CARTESIAN_POINT('',(-45.5673301698183,-89.5,15.6978257430375));
#14624=CARTESIAN_POINT('Origin',(-24.92755355845,-90.,16.1978257430375));
#14625=CARTESIAN_POINT('',(-24.92755355845,-90.,15.6978257430375));
#14626=CARTESIAN_POINT('',(-25.2811069490433,-90.,16.5513791336308));
#14627=CARTESIAN_POINT('Origin',(19.4326698301817,89.5,15.1978257430375));
#14628=CARTESIAN_POINT('',(19.4326698301817,89.5,15.6978257430375));
#14629=CARTESIAN_POINT('Origin',(-19.5453000725091,89.5,7.84891287151875));
#14630=CARTESIAN_POINT('',(-19.045300072509,89.5,7.84891287151875));
#14631=CARTESIAN_POINT('Origin',(22.9773499637455,89.5,3.19782574303749));
#14632=CARTESIAN_POINT('',(22.9773499637455,89.5,3.69782574303749));
#14633=CARTESIAN_POINT('Origin',(64.5,-45.,19.5));
#14634=CARTESIAN_POINT('',(64.5,-45.,20.));
#14635=CARTESIAN_POINT('Origin',(-32.5,-89.5,19.5));
#14636=CARTESIAN_POINT('',(-32.5,-89.5,20.));
#14637=CARTESIAN_POINT('Origin',(32.5,89.5,19.5));
#14638=CARTESIAN_POINT('',(32.5,89.5,20.));
#14639=CARTESIAN_POINT('Origin',(22.0741207385024,89.5,1.84891287151875));
#14640=CARTESIAN_POINT('',(21.5741207385024,89.5,1.84891287151875));
#14641=CARTESIAN_POINT('Origin',(43.2870603692512,89.5,15.1978257430375));
#14642=CARTESIAN_POINT('',(43.2870603692512,89.5,15.6978257430375));
#14643=CARTESIAN_POINT('Origin',(44.3272645584125,-90.,16.1978257430375));
#14644=CARTESIAN_POINT('',(44.8272645584125,-90.,16.1978257430375));
#14645=CARTESIAN_POINT('',(44.3272645584125,-90.,15.6978257430375));
#14646=CARTESIAN_POINT('Origin',(0.,0.,0.));
#14647=CARTESIAN_POINT('Origin',(44.8272645584125,-90.,15.6978257430375));
#14648=CARTESIAN_POINT('Origin',(21.5741207385024,-90.,15.6978257430375));
#14649=CARTESIAN_POINT('Origin',(21.5741207385024,-90.,3.69782574303749));
#14650=CARTESIAN_POINT('Origin',(-19.045300072509,-90.,3.69782574303749));
#14651=CARTESIAN_POINT('Origin',(-19.045300072509,-90.,15.6978257430375));
#14652=CARTESIAN_POINT('Origin',(-26.1346603396366,-90.,15.6978257430375));
#14653=CARTESIAN_POINT('Origin',(-65.,90.,0.));
#14654=CARTESIAN_POINT('Origin',(-21.8324860826741,-90.,20.));
#14655=CARTESIAN_POINT('Origin',(0.,0.,20.));
#14656=CARTESIAN_POINT('Origin',(0.,0.,20.));
#14657=CARTESIAN_POINT('',(0.,0.,0.));
#14658=CARTESIAN_POINT('Origin',(-29.5614402453126,-77.3500535736325,32.));
#14659=CARTESIAN_POINT('',(-23.5614402453126,-77.3500535736325,32.));
#14660=CARTESIAN_POINT('Origin',(-29.5614402453126,-77.3500535736325,32.));
#14661=CARTESIAN_POINT('',(-23.5614402453126,-77.3500535736325,20.));
#14662=CARTESIAN_POINT('',(-23.5614402453126,-77.3500535736325,32.));
#14663=CARTESIAN_POINT('Origin',(-29.5614402453126,-77.3500535736325,20.));
#14664=CARTESIAN_POINT('Origin',(29.5614402453126,77.3500535736325,32.));
#14665=CARTESIAN_POINT('',(35.5614402453126,77.3500535736325,32.));
#14666=CARTESIAN_POINT('Origin',(29.5614402453126,77.3500535736325,32.));
#14667=CARTESIAN_POINT('',(35.5614402453126,77.3500535736325,20.));
#14668=CARTESIAN_POINT('',(35.5614402453126,77.3500535736325,32.));
#14669=CARTESIAN_POINT('Origin',(29.5614402453126,77.3500535736325,20.));
#14670=CARTESIAN_POINT('Origin',(29.5614402453126,77.3500535736325,20.));
#14671=CARTESIAN_POINT('Origin',(29.5614402453126,-77.3500535736325,32.));
#14672=CARTESIAN_POINT('',(35.5614402453126,-77.3500535736325,32.));
#14673=CARTESIAN_POINT('Origin',(29.5614402453126,-77.3500535736325,32.));
#14674=CARTESIAN_POINT('',(35.5614402453126,-77.3500535736325,20.));
#14675=CARTESIAN_POINT('',(35.5614402453126,-77.3500535736325,32.));
#14676=CARTESIAN_POINT('Origin',(29.5614402453126,-77.3500535736325,20.));
#14677=CARTESIAN_POINT('Origin',(29.5614402453126,-77.3500535736325,20.));
#14678=CARTESIAN_POINT('Origin',(-29.5614402453126,77.3500535736325,32.));
#14679=CARTESIAN_POINT('',(-23.5614402453126,77.3500535736325,32.));
#14680=CARTESIAN_POINT('Origin',(-29.5614402453126,77.3500535736325,32.));
#14681=CARTESIAN_POINT('',(-23.5614402453126,77.3500535736325,20.));
#14682=CARTESIAN_POINT('',(-23.5614402453126,77.3500535736325,32.));
#14683=CARTESIAN_POINT('Origin',(-29.5614402453126,77.3500535736325,20.));
#14684=CARTESIAN_POINT('Origin',(-24.92755355845,89.5,16.1978257430375));
#14685=CARTESIAN_POINT('',(-25.2811069490433,89.5,16.5513791336308));
#14686=CARTESIAN_POINT('',(-24.92755355845,89.5,15.6978257430375));
#14687=CARTESIAN_POINT('Origin',(-24.92755355845,89.5,16.1978257430375));
#14688=CARTESIAN_POINT('',(-24.92755355845,90.,16.1978257430375));
#14689=CARTESIAN_POINT('Origin',(-24.92755355845,89.5,16.1978257430375));
#14690=CARTESIAN_POINT('Origin',(-24.92755355845,89.5,16.1978257430375));
#14691=CARTESIAN_POINT('Origin',(-24.92755355845,-89.5,16.1978257430375));
#14692=CARTESIAN_POINT('',(-24.92755355845,-90.,16.1978257430375));
#14693=CARTESIAN_POINT('',(-24.92755355845,-89.5,15.6978257430375));
#14694=CARTESIAN_POINT('Origin',(-24.92755355845,-89.5,16.1978257430375));
#14695=CARTESIAN_POINT('',(-25.2811069490433,-89.5,16.5513791336308));
#14696=CARTESIAN_POINT('Origin',(-24.92755355845,-89.5,16.1978257430375));
#14697=CARTESIAN_POINT('Origin',(-24.92755355845,-89.5,16.1978257430375));
#14698=CARTESIAN_POINT('Origin',(-19.545300072509,89.5,15.1978257430375));
#14699=CARTESIAN_POINT('',(-19.545300072509,89.5,15.6978257430375));
#14700=CARTESIAN_POINT('',(-19.045300072509,89.5,15.1978257430375));
#14701=CARTESIAN_POINT('Origin',(-19.545300072509,89.5,15.1978257430375));
#14702=CARTESIAN_POINT('',(-19.545300072509,90.,16.1978257430375));
#14703=CARTESIAN_POINT('Origin',(-19.545300072509,89.5,16.1978257430375));
#14704=CARTESIAN_POINT('',(-18.545300072509,90.,15.1978257430375));
#14705=CARTESIAN_POINT('Origin',(-19.545300072509,90.,15.1978257430375));
#14706=CARTESIAN_POINT('Origin',(-18.545300072509,89.5,15.1978257430375));
#14707=CARTESIAN_POINT('Origin',(19.4326698301817,89.5,16.1978257430375));
#14708=CARTESIAN_POINT('',(19.4326698301817,89.5,15.6978257430375));
#14709=CARTESIAN_POINT('',(19.4326698301817,90.,16.1978257430375));
#14710=CARTESIAN_POINT('Origin',(-23.0395928638606,89.5,19.5));
#14711=CARTESIAN_POINT('',(-23.0395928638606,90.,20.5));
#14712=CARTESIAN_POINT('',(-22.3324860826741,90.,18.7928932188135));
#14713=CARTESIAN_POINT('Origin',(-23.0395928638606,90.,19.5));
#14714=CARTESIAN_POINT('',(-22.6860394732673,89.5,19.1464466094067));
#14715=CARTESIAN_POINT('Origin',(-22.3324860826741,89.5,18.7928932188135));
#14716=CARTESIAN_POINT('',(-23.0395928638606,89.5,20.));
#14717=CARTESIAN_POINT('Origin',(-23.0395928638606,89.5,19.5));
#14718=CARTESIAN_POINT('Origin',(-23.0395928638606,89.5,20.5));
#14719=CARTESIAN_POINT('Origin',(-19.545300072509,-89.5,15.1978257430375));
#14720=CARTESIAN_POINT('',(-19.045300072509,-89.5,15.1978257430375));
#14721=CARTESIAN_POINT('',(-19.545300072509,-89.5,15.6978257430375));
#14722=CARTESIAN_POINT('Origin',(-19.545300072509,-89.5,15.1978257430375));
#14723=CARTESIAN_POINT('',(-18.545300072509,-90.,15.1978257430375));
#14724=CARTESIAN_POINT('Origin',(-18.545300072509,-89.5,15.1978257430375));
#14725=CARTESIAN_POINT('',(-19.545300072509,-90.,16.1978257430375));
#14726=CARTESIAN_POINT('Origin',(-19.545300072509,-90.,15.1978257430375));
#14727=CARTESIAN_POINT('Origin',(-19.545300072509,-89.5,16.1978257430375));
#14728=CARTESIAN_POINT('Origin',(-23.0395928638606,-89.5,19.5));
#14729=CARTESIAN_POINT('',(-22.3324860826741,-90.,18.7928932188135));
#14730=CARTESIAN_POINT('',(-23.0395928638606,-90.,20.5));
#14731=CARTESIAN_POINT('Origin',(-23.0395928638606,-90.,19.5));
#14732=CARTESIAN_POINT('',(-23.0395928638606,-89.5,20.));
#14733=CARTESIAN_POINT('Origin',(-23.0395928638606,-89.5,20.5));
#14734=CARTESIAN_POINT('',(-22.6860394732673,-89.5,19.1464466094067));
#14735=CARTESIAN_POINT('Origin',(-23.0395928638606,-89.5,19.5));
#14736=CARTESIAN_POINT('Origin',(-22.3324860826741,-89.5,18.7928932188135));
#14737=CARTESIAN_POINT('Origin',(-32.2708111714123,-89.5,8.85456813007524));
#14738=CARTESIAN_POINT('',(-32.6243645620056,-89.5,9.20812152066852));
#14739=CARTESIAN_POINT('',(-32.2708111714123,-90.,8.85456813007524));
#14740=CARTESIAN_POINT('Origin',(-18.545300072509,89.5,4.19782574303749));
#14741=CARTESIAN_POINT('',(-19.045300072509,89.5,4.19782574303749));
#14742=CARTESIAN_POINT('',(-18.545300072509,89.5,3.69782574303749));
#14743=CARTESIAN_POINT('Origin',(-18.545300072509,89.5,4.19782574303749));
#14744=CARTESIAN_POINT('',(-18.545300072509,90.,4.19782574303749));
#14745=CARTESIAN_POINT('Origin',(-18.545300072509,89.5,4.19782574303749));
#14746=CARTESIAN_POINT('Origin',(-18.545300072509,89.5,4.19782574303749));
#14747=CARTESIAN_POINT('Origin',(-18.545300072509,89.5,17.8489128715187));
#14748=CARTESIAN_POINT('',(-19.045300072509,89.5,17.8489128715187));
#14749=CARTESIAN_POINT('',(-18.545300072509,90.,17.8489128715187));
#14750=CARTESIAN_POINT('Origin',(-64.5,89.5,20.5));
#14751=CARTESIAN_POINT('',(-64.5,90.,20.5));
#14752=CARTESIAN_POINT('',(-65.,89.5,20.5));
#14753=CARTESIAN_POINT('Origin',(-64.5,89.5,20.5));
#14754=CARTESIAN_POINT('',(-64.5,89.5,20.));
#14755=CARTESIAN_POINT('Origin',(-64.5,89.5,20.5));
#14756=CARTESIAN_POINT('Origin',(-64.5,89.5,20.5));
#14757=CARTESIAN_POINT('Origin',(32.5,89.5,20.5));
#14758=CARTESIAN_POINT('',(32.5,90.,20.5));
#14759=CARTESIAN_POINT('',(32.5,89.5,20.));
#14760=CARTESIAN_POINT('Origin',(-18.545300072509,-89.5,4.19782574303749));
#14761=CARTESIAN_POINT('',(-18.545300072509,-89.5,3.69782574303749));
#14762=CARTESIAN_POINT('',(-19.045300072509,-89.5,4.19782574303749));
#14763=CARTESIAN_POINT('Origin',(-18.545300072509,-89.5,4.19782574303749));
#14764=CARTESIAN_POINT('',(-18.545300072509,-90.,4.19782574303749));
#14765=CARTESIAN_POINT('Origin',(-18.545300072509,-89.5,4.19782574303749));
#14766=CARTESIAN_POINT('Origin',(-18.545300072509,-89.5,4.19782574303749));
#14767=CARTESIAN_POINT('Origin',(-64.5,-89.5,20.5));
#14768=CARTESIAN_POINT('',(-64.5,-89.5,20.));
#14769=CARTESIAN_POINT('',(-65.,-89.5,20.5));
#14770=CARTESIAN_POINT('Origin',(-64.5,-89.5,20.5));
#14771=CARTESIAN_POINT('',(-64.5,-90.,20.5));
#14772=CARTESIAN_POINT('Origin',(-64.5,-89.5,20.5));
#14773=CARTESIAN_POINT('Origin',(-64.5,-89.5,20.5));
#14774=CARTESIAN_POINT('Origin',(-32.5,-89.5,20.5));
#14775=CARTESIAN_POINT('',(-32.5,-90.,20.5));
#14776=CARTESIAN_POINT('',(-32.5,-89.5,20.));
#14777=CARTESIAN_POINT('Origin',(21.0741207385024,89.5,4.19782574303749));
#14778=CARTESIAN_POINT('',(21.0741207385024,89.5,3.69782574303749));
#14779=CARTESIAN_POINT('',(21.5741207385024,89.5,4.19782574303749));
#14780=CARTESIAN_POINT('Origin',(21.0741207385024,89.5,4.19782574303749));
#14781=CARTESIAN_POINT('',(21.0741207385024,90.,4.19782574303749));
#14782=CARTESIAN_POINT('Origin',(21.0741207385024,89.5,4.19782574303749));
#14783=CARTESIAN_POINT('Origin',(21.0741207385024,89.5,4.19782574303749));
#14784=CARTESIAN_POINT('Origin',(22.9773499637455,89.5,4.19782574303749));
#14785=CARTESIAN_POINT('',(22.9773499637455,89.5,3.69782574303749));
#14786=CARTESIAN_POINT('',(22.9773499637455,90.,4.19782574303749));
#14787=CARTESIAN_POINT('Origin',(-64.5,89.5,31.5));
#14788=CARTESIAN_POINT('',(-64.5,90.,31.5));
#14789=CARTESIAN_POINT('',(-64.5,89.5,32.));
#14790=CARTESIAN_POINT('Origin',(-64.5,89.5,31.5));
#14791=CARTESIAN_POINT('',(-65.,89.5,31.5));
#14792=CARTESIAN_POINT('Origin',(-64.5,89.5,31.5));
#14793=CARTESIAN_POINT('Origin',(-64.5,89.5,31.5));
#14794=CARTESIAN_POINT('Origin',(-64.5,89.5,20.));
#14795=CARTESIAN_POINT('',(-64.5,90.,20.));
#14796=CARTESIAN_POINT('',(-65.,89.5,20.));
#14797=CARTESIAN_POINT('Origin',(21.0741207385024,-89.5,4.19782574303749));
#14798=CARTESIAN_POINT('',(21.5741207385024,-89.5,4.19782574303749));
#14799=CARTESIAN_POINT('',(21.0741207385024,-89.5,3.69782574303749));
#14800=CARTESIAN_POINT('Origin',(21.0741207385024,-89.5,4.19782574303749));
#14801=CARTESIAN_POINT('',(21.0741207385024,-90.,4.19782574303749));
#14802=CARTESIAN_POINT('Origin',(21.0741207385024,-89.5,4.19782574303749));
#14803=CARTESIAN_POINT('Origin',(21.0741207385024,-89.5,4.19782574303749));
#14804=CARTESIAN_POINT('Origin',(-64.5,-89.5,31.5));
#14805=CARTESIAN_POINT('',(-65.,-89.5,31.5));
#14806=CARTESIAN_POINT('',(-64.5,-89.5,32.));
#14807=CARTESIAN_POINT('Origin',(-64.5,-89.5,31.5));
#14808=CARTESIAN_POINT('',(-64.5,-90.,31.5));
#14809=CARTESIAN_POINT('Origin',(-64.5,-89.5,31.5));
#14810=CARTESIAN_POINT('Origin',(-64.5,-89.5,31.5));
#14811=CARTESIAN_POINT('Origin',(-64.5,-89.5,20.));
#14812=CARTESIAN_POINT('',(-65.,-89.5,20.));
#14813=CARTESIAN_POINT('',(-64.5,-90.,20.));
#14814=CARTESIAN_POINT('Origin',(22.0741207385024,89.5,15.1978257430375));
#14815=CARTESIAN_POINT('',(21.5741207385024,89.5,15.1978257430375));
#14816=CARTESIAN_POINT('',(22.0741207385024,89.5,15.6978257430375));
#14817=CARTESIAN_POINT('Origin',(22.0741207385024,89.5,15.1978257430375));
#14818=CARTESIAN_POINT('',(21.0741207385024,90.,15.1978257430375));
#14819=CARTESIAN_POINT('Origin',(21.0741207385024,89.5,15.1978257430375));
#14820=CARTESIAN_POINT('',(22.0741207385024,90.,16.1978257430375));
#14821=CARTESIAN_POINT('Origin',(22.0741207385024,90.,15.1978257430375));
#14822=CARTESIAN_POINT('Origin',(22.0741207385024,89.5,16.1978257430375));
#14823=CARTESIAN_POINT('Origin',(21.0741207385024,89.5,11.8489128715187));
#14824=CARTESIAN_POINT('',(21.5741207385024,89.5,11.8489128715187));
#14825=CARTESIAN_POINT('',(21.0741207385024,90.,11.8489128715187));
#14826=CARTESIAN_POINT('Origin',(64.5,89.5,31.5));
#14827=CARTESIAN_POINT('',(65.,89.5,31.5));
#14828=CARTESIAN_POINT('',(64.5,89.5,32.));
#14829=CARTESIAN_POINT('Origin',(64.5,89.5,31.5));
#14830=CARTESIAN_POINT('',(64.5,90.,31.5));
#14831=CARTESIAN_POINT('Origin',(64.5,89.5,31.5));
#14832=CARTESIAN_POINT('Origin',(64.5,89.5,31.5));
#14833=CARTESIAN_POINT('Origin',(22.0741207385024,-89.5,15.1978257430375));
#14834=CARTESIAN_POINT('',(22.0741207385024,-89.5,15.6978257430375));
#14835=CARTESIAN_POINT('',(21.5741207385024,-89.5,15.1978257430375));
#14836=CARTESIAN_POINT('Origin',(22.0741207385024,-89.5,15.1978257430375));
#14837=CARTESIAN_POINT('',(22.0741207385024,-90.,16.1978257430375));
#14838=CARTESIAN_POINT('Origin',(22.0741207385024,-89.5,16.1978257430375));
#14839=CARTESIAN_POINT('',(21.0741207385024,-90.,15.1978257430375));
#14840=CARTESIAN_POINT('Origin',(22.0741207385024,-90.,15.1978257430375));
#14841=CARTESIAN_POINT('Origin',(21.0741207385024,-89.5,15.1978257430375));
#14842=CARTESIAN_POINT('Origin',(64.5,-89.5,31.5));
#14843=CARTESIAN_POINT('',(64.5,-90.,31.5));
#14844=CARTESIAN_POINT('',(64.5,-89.5,32.));
#14845=CARTESIAN_POINT('Origin',(64.5,-89.5,31.5));
#14846=CARTESIAN_POINT('',(65.,-89.5,31.5));
#14847=CARTESIAN_POINT('Origin',(64.5,-89.5,31.5));
#14848=CARTESIAN_POINT('Origin',(64.5,-89.5,31.5));
#14849=CARTESIAN_POINT('Origin',(44.3272645584124,89.5,16.1978257430375));
#14850=CARTESIAN_POINT('',(44.3272645584125,89.5,15.6978257430375));
#14851=CARTESIAN_POINT('',(44.8272645584125,89.5,16.1978257430375));
#14852=CARTESIAN_POINT('Origin',(44.3272645584125,89.5,16.1978257430375));
#14853=CARTESIAN_POINT('',(44.3272645584124,90.,16.1978257430375));
#14854=CARTESIAN_POINT('Origin',(44.3272645584124,89.5,16.1978257430375));
#14855=CARTESIAN_POINT('Origin',(44.3272645584124,89.5,16.1978257430375));
#14856=CARTESIAN_POINT('Origin',(43.2870603692512,89.5,16.1978257430375));
#14857=CARTESIAN_POINT('',(43.2870603692512,89.5,15.6978257430375));
#14858=CARTESIAN_POINT('',(43.2870603692512,90.,16.1978257430375));
#14859=CARTESIAN_POINT('Origin',(64.5,89.5,20.5));
#14860=CARTESIAN_POINT('',(65.,89.5,20.5));
#14861=CARTESIAN_POINT('',(64.5,90.,20.5));
#14862=CARTESIAN_POINT('Origin',(64.5,89.5,20.5));
#14863=CARTESIAN_POINT('',(64.5,89.5,20.));
#14864=CARTESIAN_POINT('Origin',(64.5,89.5,20.5));
#14865=CARTESIAN_POINT('Origin',(64.5,89.5,20.5));
#14866=CARTESIAN_POINT('Origin',(44.3272645584124,-89.5,16.1978257430375));
#14867=CARTESIAN_POINT('',(44.8272645584125,-89.5,16.1978257430375));
#14868=CARTESIAN_POINT('',(44.3272645584125,-89.5,15.6978257430375));
#14869=CARTESIAN_POINT('Origin',(44.3272645584125,-89.5,16.1978257430375));
#14870=CARTESIAN_POINT('',(44.3272645584124,-90.,16.1978257430375));
#14871=CARTESIAN_POINT('Origin',(44.3272645584124,-89.5,16.1978257430375));
#14872=CARTESIAN_POINT('Origin',(44.3272645584124,-89.5,16.1978257430375));
#14873=CARTESIAN_POINT('Origin',(64.5,-89.5,20.5));
#14874=CARTESIAN_POINT('',(64.5,-90.,20.5));
#14875=CARTESIAN_POINT('',(65.,-89.5,20.5));
#14876=CARTESIAN_POINT('Origin',(64.5,-89.5,20.5));
#14877=CARTESIAN_POINT('',(64.5,-89.5,20.));
#14878=CARTESIAN_POINT('Origin',(64.5,-89.5,20.5));
#14879=CARTESIAN_POINT('Origin',(64.5,-89.5,20.5));
#14880=CARTESIAN_POINT('Origin',(45.3272645584125,89.5,19.5));
#14881=CARTESIAN_POINT('',(44.8272645584125,89.5,19.5));
#14882=CARTESIAN_POINT('',(45.3272645584125,89.5,20.));
#14883=CARTESIAN_POINT('Origin',(45.3272645584125,89.5,19.5));
#14884=CARTESIAN_POINT('',(44.3272645584124,90.,19.5));
#14885=CARTESIAN_POINT('Origin',(44.3272645584124,89.5,19.5));
#14886=CARTESIAN_POINT('',(45.3272645584125,90.,20.5));
#14887=CARTESIAN_POINT('Origin',(45.3272645584125,90.,19.5));
#14888=CARTESIAN_POINT('Origin',(45.3272645584125,89.5,20.5));
#14889=CARTESIAN_POINT('Origin',(44.3272645584124,89.5,17.8489128715187));
#14890=CARTESIAN_POINT('',(44.8272645584125,89.5,17.8489128715187));
#14891=CARTESIAN_POINT('',(44.3272645584124,90.,17.8489128715187));
#14892=CARTESIAN_POINT('Origin',(32.5,89.5,20.5));
#14893=CARTESIAN_POINT('',(32.5,90.,20.5));
#14894=CARTESIAN_POINT('',(32.5,89.5,20.));
#14895=CARTESIAN_POINT('Origin',(45.3272645584125,-89.5,19.5));
#14896=CARTESIAN_POINT('',(45.3272645584125,-89.5,20.));
#14897=CARTESIAN_POINT('',(44.8272645584125,-89.5,19.5));
#14898=CARTESIAN_POINT('Origin',(45.3272645584125,-89.5,19.5));
#14899=CARTESIAN_POINT('',(45.3272645584125,-90.,20.5));
#14900=CARTESIAN_POINT('Origin',(45.3272645584125,-89.5,20.5));
#14901=CARTESIAN_POINT('',(44.3272645584124,-90.,19.5));
#14902=CARTESIAN_POINT('Origin',(45.3272645584125,-90.,19.5));
#14903=CARTESIAN_POINT('Origin',(44.3272645584124,-89.5,19.5));
#14904=CARTESIAN_POINT('Origin',(-32.5,-89.5,20.5));
#14905=CARTESIAN_POINT('',(-32.5,-90.,20.5));
#14906=CARTESIAN_POINT('',(-32.5,-89.5,20.));
#14907=CARTESIAN_POINT('Origin',(44.3272645584124,-89.5,17.8489128715187));
#14908=CARTESIAN_POINT('',(44.8272645584125,-89.5,17.8489128715187));
#14909=CARTESIAN_POINT('',(44.3272645584124,-90.,17.8489128715187));
#14910=CARTESIAN_POINT('Origin',(45.3272645584125,-45.,19.5));
#14911=CARTESIAN_POINT('',(45.3272645584125,-45.,20.));
#14912=CARTESIAN_POINT('',(44.8272645584125,-45.,19.5));
#14913=CARTESIAN_POINT('Origin',(64.5,-45.,20.5));
#14914=CARTESIAN_POINT('',(65.,-45.,20.5));
#14915=CARTESIAN_POINT('',(64.5,-45.,20.));
#14916=CARTESIAN_POINT('Origin',(64.5,-89.5,20.));
#14917=CARTESIAN_POINT('',(64.5,-90.,20.));
#14918=CARTESIAN_POINT('',(65.,-89.5,20.));
#14919=CARTESIAN_POINT('Origin',(-21.7129396307488,-89.5,16.1978257430375));
#14920=CARTESIAN_POINT('',(-21.7129396307488,-89.5,15.6978257430375));
#14921=CARTESIAN_POINT('',(-21.7129396307488,-90.,16.1978257430375));
#14922=CARTESIAN_POINT('Origin',(44.3272645584125,-90.,16.1978257430375));
#14923=CARTESIAN_POINT('',(44.3272645584125,-90.,15.6978257430375));
#14924=CARTESIAN_POINT('',(44.8272645584125,-90.,16.1978257430375));
#14925=CARTESIAN_POINT('Origin',(64.5,89.5,20.));
#14926=CARTESIAN_POINT('',(65.,89.5,20.));
#14927=CARTESIAN_POINT('',(64.5,90.,20.));
#14928=CARTESIAN_POINT('Origin',(64.5,-45.,31.5));
#14929=CARTESIAN_POINT('',(64.5,-45.,32.));
#14930=CARTESIAN_POINT('',(65.,-45.,31.5));
#14931=CARTESIAN_POINT('Origin',(-32.5,-89.5,31.5));
#14932=CARTESIAN_POINT('',(-32.5,-89.5,32.));
#14933=CARTESIAN_POINT('',(-32.5,-90.,31.5));
#14934=CARTESIAN_POINT('Origin',(21.0741207385024,-89.5,11.8489128715187));
#14935=CARTESIAN_POINT('',(21.5741207385024,-89.5,11.8489128715187));
#14936=CARTESIAN_POINT('',(21.0741207385024,-90.,11.8489128715187));
#14937=CARTESIAN_POINT('Origin',(22.0741207385024,-90.,15.1978257430375));
#14938=CARTESIAN_POINT('',(21.5741207385024,-90.,15.1978257430375));
#14939=CARTESIAN_POINT('',(22.0741207385024,-90.,15.6978257430375));
#14940=CARTESIAN_POINT('Origin',(32.5,89.5,31.5));
#14941=CARTESIAN_POINT('',(32.5,89.5,32.));
#14942=CARTESIAN_POINT('',(32.5,90.,31.5));
#14943=CARTESIAN_POINT('Origin',(-64.5,45.,31.5));
#14944=CARTESIAN_POINT('',(-64.5,45.,32.));
#14945=CARTESIAN_POINT('',(-65.,45.,31.5));
#14946=CARTESIAN_POINT('Origin',(-42.0226500362545,-89.5,4.19782574303749));
#14947=CARTESIAN_POINT('',(-42.0226500362545,-89.5,3.69782574303749));
#14948=CARTESIAN_POINT('',(-42.0226500362545,-90.,4.19782574303749));
#14949=CARTESIAN_POINT('Origin',(21.0741207385024,-90.,4.19782574303749));
#14950=CARTESIAN_POINT('',(21.0741207385024,-90.,3.69782574303749));
#14951=CARTESIAN_POINT('',(21.5741207385024,-90.,4.19782574303749));
#14952=CARTESIAN_POINT('Origin',(-64.5,45.,20.5));
#14953=CARTESIAN_POINT('',(-65.,45.,20.5));
#14954=CARTESIAN_POINT('',(-64.5,45.,20.));
#14955=CARTESIAN_POINT('Origin',(-18.545300072509,-89.5,17.8489128715187));
#14956=CARTESIAN_POINT('',(-19.045300072509,-89.5,17.8489128715187));
#14957=CARTESIAN_POINT('',(-18.545300072509,-90.,17.8489128715187));
#14958=CARTESIAN_POINT('Origin',(-18.545300072509,-90.,4.19782574303749));
#14959=CARTESIAN_POINT('',(-19.045300072509,-90.,4.19782574303749));
#14960=CARTESIAN_POINT('',(-18.545300072509,-90.,3.69782574303749));
#14961=CARTESIAN_POINT('Origin',(-23.0395928638606,-45.,19.5));
#14962=CARTESIAN_POINT('',(-23.0395928638606,-45.,20.));
#14963=CARTESIAN_POINT('',(-22.6860394732673,-45.,19.1464466094067));
#14964=CARTESIAN_POINT('Origin',(-45.5673301698183,-89.5,16.1978257430375));
#14965=CARTESIAN_POINT('',(-45.5673301698183,-89.5,15.6978257430375));
#14966=CARTESIAN_POINT('',(-45.5673301698183,-90.,16.1978257430375));
#14967=CARTESIAN_POINT('Origin',(-19.545300072509,-90.,15.1978257430375));
#14968=CARTESIAN_POINT('',(-19.545300072509,-90.,15.6978257430375));
#14969=CARTESIAN_POINT('',(-19.045300072509,-90.,15.1978257430375));
#14970=CARTESIAN_POINT('Origin',(0.229188828587721,89.5,41.3545681300752));
#14971=CARTESIAN_POINT('',(-0.124364562005555,89.5,41.7081215206685));
#14972=CARTESIAN_POINT('',(0.229188828587721,90.,41.3545681300752));
#14973=CARTESIAN_POINT('Origin',(-24.92755355845,-90.,16.1978257430375));
#14974=CARTESIAN_POINT('',(-25.2811069490433,-90.,16.5513791336308));
#14975=CARTESIAN_POINT('',(-24.92755355845,-90.,15.6978257430375));
#14976=CARTESIAN_POINT('Origin',(-65.,-90.,20.));
#14977=CARTESIAN_POINT('Origin',(-21.8324860826741,-90.,20.));
#14978=CARTESIAN_POINT('Origin',(0.,0.,20.));
#14979=CARTESIAN_POINT('Origin',(-65.,90.,20.));
#14980=CARTESIAN_POINT('Origin',(0.,0.,20.));
#14981=CARTESIAN_POINT('Origin',(44.8272645584125,-90.,15.6978257430375));
#14982=CARTESIAN_POINT('Origin',(65.,-90.,20.));
#14983=CARTESIAN_POINT('Origin',(21.5741207385024,-90.,15.6978257430375));
#14984=CARTESIAN_POINT('Origin',(0.,0.,32.));
#14985=CARTESIAN_POINT('Origin',(21.5741207385024,-90.,3.69782574303749));
#14986=CARTESIAN_POINT('Origin',(-19.045300072509,-90.,3.69782574303749));
#14987=CARTESIAN_POINT('Origin',(-19.045300072509,-90.,15.6978257430375));
#14988=CARTESIAN_POINT('Origin',(-26.1346603396366,-90.,15.6978257430375));
#14989=CARTESIAN_POINT('Origin',(65.,90.,20.));
#14990=CARTESIAN_POINT('',(0.,0.,0.));
#14991=CARTESIAN_POINT('Origin',(37.3901590350027,65.,45.9189319234316));
#14992=CARTESIAN_POINT('',(33.3901590350027,65.,45.9189319234316));
#14993=CARTESIAN_POINT('Origin',(37.3901590350027,65.,45.9189319234316));
#14994=CARTESIAN_POINT('',(33.3901590350027,49.,45.9189319234316));
#14995=CARTESIAN_POINT('',(33.3901590350027,65.,45.9189319234316));
#14996=CARTESIAN_POINT('Origin',(37.3901590350027,49.,45.9189319234316));
#14997=CARTESIAN_POINT('Origin',(37.3901590350027,49.,45.9189319234316));
#14998=CARTESIAN_POINT('Origin',(-37.3901590350027,65.,45.9189319234316));
#14999=CARTESIAN_POINT('',(-41.3901590350027,65.,45.9189319234316));
#15000=CARTESIAN_POINT('Origin',(-37.3901590350027,65.,45.9189319234316));
#15001=CARTESIAN_POINT('',(-41.3901590350027,49.,45.9189319234316));
#15002=CARTESIAN_POINT('',(-41.3901590350027,65.,45.9189319234316));
#15003=CARTESIAN_POINT('Origin',(-37.3901590350027,49.,45.9189319234316));
#15004=CARTESIAN_POINT('Origin',(-37.3901590350027,49.,45.9189319234316));
#15005=CARTESIAN_POINT('Origin',(-77.3901590350027,65.,45.9189319234316));
#15006=CARTESIAN_POINT('',(-81.3901590350027,65.,45.9189319234316));
#15007=CARTESIAN_POINT('Origin',(-77.3901590350027,65.,45.9189319234316));
#15008=CARTESIAN_POINT('',(-81.3901590350027,49.,45.9189319234316));
#15009=CARTESIAN_POINT('',(-81.3901590350027,65.,45.9189319234316));
#15010=CARTESIAN_POINT('Origin',(-77.3901590350027,49.,45.9189319234316));
#15011=CARTESIAN_POINT('Origin',(-77.3901590350027,49.,45.9189319234316));
#15012=CARTESIAN_POINT('Origin',(77.3901590350027,65.,45.9189319234316));
#15013=CARTESIAN_POINT('',(73.3901590350027,65.,45.9189319234316));
#15014=CARTESIAN_POINT('Origin',(77.3901590350027,65.,45.9189319234316));
#15015=CARTESIAN_POINT('',(73.3901590350027,49.,45.9189319234316));
#15016=CARTESIAN_POINT('',(73.3901590350027,65.,45.9189319234316));
#15017=CARTESIAN_POINT('Origin',(77.3901590350027,49.,45.9189319234316));
#15018=CARTESIAN_POINT('Origin',(77.3901590350027,49.,45.9189319234316));
#15019=CARTESIAN_POINT('Origin',(-37.3901590350027,-65.,45.9189319234316));
#15020=CARTESIAN_POINT('',(-41.3901590350027,-65.,45.9189319234316));
#15021=CARTESIAN_POINT('Origin',(-37.3901590350027,-65.,45.9189319234316));
#15022=CARTESIAN_POINT('',(-41.3901590350027,-49.,45.9189319234316));
#15023=CARTESIAN_POINT('',(-41.3901590350027,-65.,45.9189319234316));
#15024=CARTESIAN_POINT('Origin',(-37.3901590350027,-49.,45.9189319234316));
#15025=CARTESIAN_POINT('Origin',(-37.3901590350027,-49.,45.9189319234316));
#15026=CARTESIAN_POINT('Origin',(77.3901590350027,-65.,45.9189319234316));
#15027=CARTESIAN_POINT('',(73.3901590350027,-65.,45.9189319234316));
#15028=CARTESIAN_POINT('Origin',(77.3901590350027,-65.,45.9189319234316));
#15029=CARTESIAN_POINT('',(73.3901590350027,-49.,45.9189319234316));
#15030=CARTESIAN_POINT('',(73.3901590350027,-65.,45.9189319234316));
#15031=CARTESIAN_POINT('Origin',(77.3901590350027,-49.,45.9189319234316));
#15032=CARTESIAN_POINT('Origin',(77.3901590350027,-49.,45.9189319234316));
#15033=CARTESIAN_POINT('Origin',(-77.3901590350027,-65.,45.9189319234316));
#15034=CARTESIAN_POINT('',(-81.3901590350027,-65.,45.9189319234316));
#15035=CARTESIAN_POINT('Origin',(-77.3901590350027,-65.,45.9189319234316));
#15036=CARTESIAN_POINT('',(-81.3901590350027,-49.,45.9189319234316));
#15037=CARTESIAN_POINT('',(-81.3901590350027,-65.,45.9189319234316));
#15038=CARTESIAN_POINT('Origin',(-77.3901590350027,-49.,45.9189319234316));
#15039=CARTESIAN_POINT('Origin',(-77.3901590350027,-49.,45.9189319234316));
#15040=CARTESIAN_POINT('Origin',(37.3901590350027,-65.,45.9189319234316));
#15041=CARTESIAN_POINT('',(33.3901590350027,-65.,45.9189319234316));
#15042=CARTESIAN_POINT('Origin',(37.3901590350027,-65.,45.9189319234316));
#15043=CARTESIAN_POINT('',(33.3901590350027,-49.,45.9189319234316));
#15044=CARTESIAN_POINT('',(33.3901590350027,-65.,45.9189319234316));
#15045=CARTESIAN_POINT('Origin',(37.3901590350027,-49.,45.9189319234316));
#15046=CARTESIAN_POINT('Origin',(37.3901590350027,-49.,45.9189319234316));
#15047=CARTESIAN_POINT('Origin',(-1.4432899320127E-14,-65.,38.2895355526966));
#15048=CARTESIAN_POINT('',(-90.,-64.5,38.2895355526966));
#15049=CARTESIAN_POINT('',(-89.5,-65.,38.2895355526966));
#15050=CARTESIAN_POINT('Origin',(-89.5,-64.5,38.2895355526966));
#15051=CARTESIAN_POINT('',(-90.,-62.,38.2895355526966));
#15052=CARTESIAN_POINT('',(-90.,1.99840144432528E-14,38.2895355526966));
#15053=CARTESIAN_POINT('',(90.,-62.,38.2895355526966));
#15054=CARTESIAN_POINT('',(-1.37667655053519E-14,-62.,38.2895355526966));
#15055=CARTESIAN_POINT('',(90.,-64.5,38.2895355526966));
#15056=CARTESIAN_POINT('',(90.,-65.,38.2895355526966));
#15057=CARTESIAN_POINT('',(89.5,-65.,38.2895355526966));
#15058=CARTESIAN_POINT('Origin',(89.5,-64.5,38.2895355526966));
#15059=CARTESIAN_POINT('',(-45.,-65.,38.2895355526966));
#15060=CARTESIAN_POINT('Origin',(-1.37667655053519E-14,-62.,34.7895355526966));
#15061=CARTESIAN_POINT('',(-89.5,-65.,34.7895355526966));
#15062=CARTESIAN_POINT('',(-90.,-64.5,34.7895355526966));
#15063=CARTESIAN_POINT('Origin',(-89.5,-64.5,34.7895355526966));
#15064=CARTESIAN_POINT('',(89.5,-65.,34.7895355526966));
#15065=CARTESIAN_POINT('',(-45.,-65.,34.7895355526966));
#15066=CARTESIAN_POINT('',(90.,-64.5,34.7895355526966));
#15067=CARTESIAN_POINT('Origin',(89.5,-64.5,34.7895355526966));
#15068=CARTESIAN_POINT('',(90.,-62.,34.7895355526966));
#15069=CARTESIAN_POINT('',(90.,-63.5,34.7895355526966));
#15070=CARTESIAN_POINT('',(-90.,-62.,34.7895355526966));
#15071=CARTESIAN_POINT('',(-1.37667655053519E-14,-62.,34.7895355526966));
#15072=CARTESIAN_POINT('',(-90.,1.50000000000002,34.7895355526966));
#15073=CARTESIAN_POINT('Origin',(-1.37667655053519E-14,-62.,38.2895355526966));
#15074=CARTESIAN_POINT('',(90.,-62.,35.1447677763483));
#15075=CARTESIAN_POINT('',(-90.,-62.,35.1447677763483));
#15076=CARTESIAN_POINT('Origin',(-89.5,-64.5,32.));
#15077=CARTESIAN_POINT('',(-90.,-64.5,32.5));
#15078=CARTESIAN_POINT('',(-90.,-64.5,32.));
#15079=CARTESIAN_POINT('',(-89.5,-65.,32.));
#15080=CARTESIAN_POINT('Origin',(-89.5,-64.5,32.5));
#15081=CARTESIAN_POINT('',(-89.5,-65.,32.));
#15082=CARTESIAN_POINT('Origin',(-89.5,-64.5,32.));
#15083=CARTESIAN_POINT('',(-89.5,-65.,51.5));
#15084=CARTESIAN_POINT('',(-89.5,-65.,32.));
#15085=CARTESIAN_POINT('',(-90.,-64.5,51.5));
#15086=CARTESIAN_POINT('Origin',(-89.5,-64.5,51.5));
#15087=CARTESIAN_POINT('',(-90.,-64.5,32.));
#15088=CARTESIAN_POINT('Origin',(-90.,-65.,32.));
#15089=CARTESIAN_POINT('',(89.5,-65.,32.));
#15090=CARTESIAN_POINT('',(-90.,-65.,32.));
#15091=CARTESIAN_POINT('',(89.5,-65.,32.));
#15092=CARTESIAN_POINT('Origin',(-90.,-65.,32.));
#15093=CARTESIAN_POINT('',(89.5,-65.,51.5));
#15094=CARTESIAN_POINT('',(89.5,-65.,32.));
#15095=CARTESIAN_POINT('',(-45.,-65.,51.5));
#15096=CARTESIAN_POINT('Origin',(89.5,-64.5,32.));
#15097=CARTESIAN_POINT('',(90.,-64.5,32.5));
#15098=CARTESIAN_POINT('Origin',(89.5,-64.5,32.5));
#15099=CARTESIAN_POINT('',(90.,-64.5,32.));
#15100=CARTESIAN_POINT('Origin',(89.5,-64.5,32.));
#15101=CARTESIAN_POINT('',(90.,-64.5,51.5));
#15102=CARTESIAN_POINT('',(90.,-64.5,32.));
#15103=CARTESIAN_POINT('Origin',(89.5,-64.5,51.5));
#15104=CARTESIAN_POINT('Origin',(90.,-65.,32.));
#15105=CARTESIAN_POINT('',(90.,64.5,32.5));
#15106=CARTESIAN_POINT('',(90.,-32.5,32.5));
#15107=CARTESIAN_POINT('',(90.,64.5,34.7895355526966));
#15108=CARTESIAN_POINT('',(90.,64.5,32.));
#15109=CARTESIAN_POINT('',(90.,62.,34.7895355526966));
#15110=CARTESIAN_POINT('',(90.,-1.50000000000002,34.7895355526966));
#15111=CARTESIAN_POINT('',(90.,62.,38.2895355526966));
#15112=CARTESIAN_POINT('',(90.,62.,35.1447677763483));
#15113=CARTESIAN_POINT('',(90.,64.5,38.2895355526966));
#15114=CARTESIAN_POINT('',(90.,-1.99840144432528E-14,38.2895355526966));
#15115=CARTESIAN_POINT('',(90.,64.5,51.5));
#15116=CARTESIAN_POINT('',(90.,64.5,32.));
#15117=CARTESIAN_POINT('',(90.,23.0395928638606,51.5));
#15118=CARTESIAN_POINT('',(90.,-32.5,51.5));
#15119=CARTESIAN_POINT('',(90.,25.6346603396366,48.904932524224));
#15120=CARTESIAN_POINT('',(90.,5.4779179525988,69.0616749112618));
#15121=CARTESIAN_POINT('',(90.,24.92755355845,47.1978257430375));
#15122=CARTESIAN_POINT('Origin',(90.,24.92755355845,48.1978257430375));
#15123=CARTESIAN_POINT('',(90.,19.545300072509,47.1978257430375));
#15124=CARTESIAN_POINT('',(90.,-19.4326698301817,47.1978257430375));
#15125=CARTESIAN_POINT('',(90.,19.545300072509,36.1978257430375));
#15126=CARTESIAN_POINT('',(90.,19.545300072509,39.8489128715187));
#15127=CARTESIAN_POINT('',(90.,18.545300072509,35.1978257430375));
#15128=CARTESIAN_POINT('Origin',(90.,18.545300072509,36.1978257430375));
#15129=CARTESIAN_POINT('',(90.,-21.0741207385024,35.1978257430375));
#15130=CARTESIAN_POINT('',(90.,-22.9773499637455,35.1978257430375));
#15131=CARTESIAN_POINT('',(90.,-22.0741207385024,36.1978257430375));
#15132=CARTESIAN_POINT('Origin',(90.,-21.0741207385024,36.1978257430375));
#15133=CARTESIAN_POINT('',(90.,-22.0741207385024,47.1978257430375));
#15134=CARTESIAN_POINT('',(90.,-22.0741207385024,33.8489128715187));
#15135=CARTESIAN_POINT('',(90.,-44.3272645584125,47.1978257430375));
#15136=CARTESIAN_POINT('',(90.,-43.2870603692512,47.1978257430375));
#15137=CARTESIAN_POINT('',(90.,-45.3272645584125,48.1978257430375));
#15138=CARTESIAN_POINT('Origin',(90.,-44.3272645584125,48.1978257430375));
#15139=CARTESIAN_POINT('',(90.,-45.3272645584125,51.5));
#15140=CARTESIAN_POINT('',(90.,-45.3272645584125,39.8489128715187));
#15141=CARTESIAN_POINT('',(90.,-32.5,51.5));
#15142=CARTESIAN_POINT('Origin',(1.4432899320127E-14,65.,38.2895355526966));
#15143=CARTESIAN_POINT('',(89.5,65.,38.2895355526966));
#15144=CARTESIAN_POINT('Origin',(89.5,64.5,38.2895355526966));
#15145=CARTESIAN_POINT('',(-90.,62.,38.2895355526966));
#15146=CARTESIAN_POINT('',(1.37667655053519E-14,62.,38.2895355526966));
#15147=CARTESIAN_POINT('',(-90.,64.5,38.2895355526966));
#15148=CARTESIAN_POINT('',(-90.,65.,38.2895355526966));
#15149=CARTESIAN_POINT('',(-89.5,65.,38.2895355526966));
#15150=CARTESIAN_POINT('Origin',(-89.5,64.5,38.2895355526966));
#15151=CARTESIAN_POINT('',(45.,65.,38.2895355526966));
#15152=CARTESIAN_POINT('Origin',(1.37667655053519E-14,62.,34.7895355526966));
#15153=CARTESIAN_POINT('',(89.5,65.,34.7895355526966));
#15154=CARTESIAN_POINT('Origin',(89.5,64.5,34.7895355526966));
#15155=CARTESIAN_POINT('',(-89.5,65.,34.7895355526966));
#15156=CARTESIAN_POINT('',(45.,65.,34.7895355526966));
#15157=CARTESIAN_POINT('',(-90.,64.5,34.7895355526966));
#15158=CARTESIAN_POINT('Origin',(-89.5,64.5,34.7895355526966));
#15159=CARTESIAN_POINT('',(-90.,62.,34.7895355526966));
#15160=CARTESIAN_POINT('',(-90.,63.5,34.7895355526966));
#15161=CARTESIAN_POINT('',(1.37667655053519E-14,62.,34.7895355526966));
#15162=CARTESIAN_POINT('Origin',(1.37667655053519E-14,62.,38.2895355526966));
#15163=CARTESIAN_POINT('',(-90.,62.,35.1447677763483));
#15164=CARTESIAN_POINT('Origin',(89.5,64.5,32.));
#15165=CARTESIAN_POINT('',(89.5,65.,51.5));
#15166=CARTESIAN_POINT('',(89.5,65.,32.));
#15167=CARTESIAN_POINT('Origin',(89.5,64.5,51.5));
#15168=CARTESIAN_POINT('Origin',(-90.,65.,32.));
#15169=CARTESIAN_POINT('',(-90.,-45.3272645584124,51.5));
#15170=CARTESIAN_POINT('',(-90.,32.5,51.5));
#15171=CARTESIAN_POINT('',(-90.,-45.3272645584124,48.1978257430375));
#15172=CARTESIAN_POINT('',(-90.,-45.3272645584124,39.8489128715187));
#15173=CARTESIAN_POINT('',(-90.,-44.3272645584124,47.1978257430375));
#15174=CARTESIAN_POINT('Origin',(-90.,-44.3272645584124,48.1978257430375));
#15175=CARTESIAN_POINT('',(-90.,-22.0741207385023,47.1978257430375));
#15176=CARTESIAN_POINT('',(-90.,21.7129396307488,47.1978257430375));
#15177=CARTESIAN_POINT('',(-90.,-22.0741207385023,36.1978257430375));
#15178=CARTESIAN_POINT('',(-90.,-22.0741207385023,33.8489128715187));
#15179=CARTESIAN_POINT('',(-90.,-21.0741207385023,35.1978257430375));
#15180=CARTESIAN_POINT('Origin',(-90.,-21.0741207385023,36.1978257430375));
#15181=CARTESIAN_POINT('',(-90.,18.5453000725091,35.1978257430375));
#15182=CARTESIAN_POINT('',(-90.,42.0226500362545,35.1978257430375));
#15183=CARTESIAN_POINT('',(-90.,19.5453000725091,36.1978257430375));
#15184=CARTESIAN_POINT('Origin',(-90.,18.5453000725091,36.1978257430375));
#15185=CARTESIAN_POINT('',(-90.,19.5453000725091,47.1978257430375));
#15186=CARTESIAN_POINT('',(-90.,19.5453000725091,39.8489128715187));
#15187=CARTESIAN_POINT('',(-90.,24.9275535584501,47.1978257430375));
#15188=CARTESIAN_POINT('',(-90.,45.5673301698183,47.1978257430375));
#15189=CARTESIAN_POINT('',(-90.,25.6346603396366,48.904932524224));
#15190=CARTESIAN_POINT('Origin',(-90.,24.9275535584501,48.1978257430375));
#15191=CARTESIAN_POINT('',(-90.,23.0395928638606,51.5));
#15192=CARTESIAN_POINT('',(-90.,37.9779179525988,36.5616749112618));
#15193=CARTESIAN_POINT('',(-90.,64.5,51.5));
#15194=CARTESIAN_POINT('',(-90.,32.5,51.5));
#15195=CARTESIAN_POINT('',(-90.,64.5,32.));
#15196=CARTESIAN_POINT('',(-90.,64.5,32.5));
#15197=CARTESIAN_POINT('',(-90.,64.5,32.));
#15198=CARTESIAN_POINT('',(-90.,32.5,32.5));
#15199=CARTESIAN_POINT('Origin',(90.,65.,32.));
#15200=CARTESIAN_POINT('',(-89.5,65.,51.5));
#15201=CARTESIAN_POINT('',(-89.5,65.,32.));
#15202=CARTESIAN_POINT('',(45.,65.,51.5));
#15203=CARTESIAN_POINT('Origin',(-89.5,64.5,32.));
#15204=CARTESIAN_POINT('',(-89.5,65.,32.5));
#15205=CARTESIAN_POINT('',(-89.5,65.,32.));
#15206=CARTESIAN_POINT('Origin',(-89.5,64.5,32.5));
#15207=CARTESIAN_POINT('Origin',(89.5,-44.3272645584125,48.1978257430375));
#15208=CARTESIAN_POINT('',(89.5,-44.3272645584125,47.6978257430375));
#15209=CARTESIAN_POINT('Origin',(89.5,-44.3272645584125,47.1978257430375));
#15210=CARTESIAN_POINT('',(89.5,-44.8272645584125,48.1978257430375));
#15211=CARTESIAN_POINT('Origin',(89.5,-44.3272645584125,48.1978257430375));
#15212=CARTESIAN_POINT('Origin',(89.5,-45.3272645584125,48.1978257430375));
#15213=CARTESIAN_POINT('Origin',(-89.5,-44.3272645584124,48.1978257430375));
#15214=CARTESIAN_POINT('',(-89.5,-44.8272645584124,48.1978257430375));
#15215=CARTESIAN_POINT('Origin',(-89.5,-45.3272645584124,48.1978257430375));
#15216=CARTESIAN_POINT('',(-89.5,-44.3272645584124,47.6978257430375));
#15217=CARTESIAN_POINT('Origin',(-89.5,-44.3272645584124,48.1978257430375));
#15218=CARTESIAN_POINT('Origin',(-89.5,-44.3272645584124,47.1978257430375));
#15219=CARTESIAN_POINT('Origin',(89.5,-22.0741207385024,47.1978257430375));
#15220=CARTESIAN_POINT('',(89.5,-22.0741207385024,47.6978257430375));
#15221=CARTESIAN_POINT('Origin',(89.5,-22.0741207385024,47.1978257430375));
#15222=CARTESIAN_POINT('',(89.5,-21.5741207385024,47.1978257430375));
#15223=CARTESIAN_POINT('Origin',(89.5,-22.0741207385024,47.1978257430375));
#15224=CARTESIAN_POINT('Origin',(89.5,-22.0741207385024,47.1978257430375));
#15225=CARTESIAN_POINT('Origin',(89.5,-45.3272645584125,51.5));
#15226=CARTESIAN_POINT('',(89.5,-45.3272645584125,52.));
#15227=CARTESIAN_POINT('Origin',(89.5,-45.3272645584125,51.5));
#15228=CARTESIAN_POINT('',(89.5,-44.8272645584125,51.5));
#15229=CARTESIAN_POINT('Origin',(89.5,-45.3272645584125,51.5));
#15230=CARTESIAN_POINT('Origin',(89.5,-45.3272645584125,51.5));
#15231=CARTESIAN_POINT('Origin',(89.5,-45.3272645584125,39.8489128715187));
#15232=CARTESIAN_POINT('',(89.5,-44.8272645584125,39.8489128715187));
#15233=CARTESIAN_POINT('Origin',(-89.5,-22.0741207385023,47.1978257430375));
#15234=CARTESIAN_POINT('',(-89.5,-21.5741207385023,47.1978257430375));
#15235=CARTESIAN_POINT('Origin',(-89.5,-22.0741207385023,47.1978257430375));
#15236=CARTESIAN_POINT('',(-89.5,-22.0741207385023,47.6978257430375));
#15237=CARTESIAN_POINT('Origin',(-89.5,-22.0741207385023,47.1978257430375));
#15238=CARTESIAN_POINT('Origin',(-89.5,-22.0741207385023,47.1978257430375));
#15239=CARTESIAN_POINT('Origin',(-89.5,21.7129396307488,47.1978257430375));
#15240=CARTESIAN_POINT('',(-89.5,21.7129396307488,47.6978257430375));
#15241=CARTESIAN_POINT('Origin',(-90.,-22.0741207385023,47.1978257430375));
#15242=CARTESIAN_POINT('',(-90.,-22.0741207385023,47.6978257430375));
#15243=CARTESIAN_POINT('',(-90.,-21.5741207385023,47.1978257430375));
#15244=CARTESIAN_POINT('Origin',(-89.5,-45.3272645584124,51.5));
#15245=CARTESIAN_POINT('',(-89.5,-45.3272645584124,52.));
#15246=CARTESIAN_POINT('Origin',(-89.5,-45.3272645584124,51.5));
#15247=CARTESIAN_POINT('',(-89.5,-44.8272645584124,51.5));
#15248=CARTESIAN_POINT('Origin',(-89.5,-45.3272645584124,51.5));
#15249=CARTESIAN_POINT('Origin',(-89.5,-45.3272645584124,51.5));
#15250=CARTESIAN_POINT('Origin',(-45.,-45.3272645584124,51.5));
#15251=CARTESIAN_POINT('',(-45.,-45.3272645584124,52.));
#15252=CARTESIAN_POINT('',(-45.,-44.8272645584124,51.5));
#15253=CARTESIAN_POINT('Origin',(-89.5,-45.3272645584124,39.8489128715187));
#15254=CARTESIAN_POINT('',(-89.5,-44.8272645584124,39.8489128715187));
#15255=CARTESIAN_POINT('Origin',(89.5,-21.0741207385024,36.1978257430375));
#15256=CARTESIAN_POINT('',(89.5,-21.0741207385024,35.6978257430375));
#15257=CARTESIAN_POINT('Origin',(89.5,-21.0741207385024,35.1978257430375));
#15258=CARTESIAN_POINT('',(89.5,-21.5741207385024,36.1978257430375));
#15259=CARTESIAN_POINT('Origin',(89.5,-21.0741207385024,36.1978257430375));
#15260=CARTESIAN_POINT('Origin',(89.5,-22.0741207385024,36.1978257430375));
#15261=CARTESIAN_POINT('Origin',(89.5,-64.5,51.5));
#15262=CARTESIAN_POINT('',(89.5,-64.5,52.));
#15263=CARTESIAN_POINT('Origin',(89.5,-64.5,51.5));
#15264=CARTESIAN_POINT('Origin',(89.5,-64.5,51.5));
#15265=CARTESIAN_POINT('Origin',(-89.5,-21.0741207385023,36.1978257430375));
#15266=CARTESIAN_POINT('',(-89.5,-21.5741207385023,36.1978257430375));
#15267=CARTESIAN_POINT('Origin',(-89.5,-22.0741207385023,36.1978257430375));
#15268=CARTESIAN_POINT('',(-89.5,-21.0741207385023,35.6978257430375));
#15269=CARTESIAN_POINT('Origin',(-89.5,-21.0741207385023,36.1978257430375));
#15270=CARTESIAN_POINT('Origin',(-89.5,-21.0741207385023,35.1978257430375));
#15271=CARTESIAN_POINT('Origin',(-89.5,-22.0741207385023,33.8489128715187));
#15272=CARTESIAN_POINT('',(-89.5,-21.5741207385023,33.8489128715187));
#15273=CARTESIAN_POINT('Origin',(-90.,-21.0741207385023,36.1978257430375));
#15274=CARTESIAN_POINT('',(-90.,-21.5741207385023,36.1978257430375));
#15275=CARTESIAN_POINT('',(-90.,-21.0741207385023,35.6978257430375));
#15276=CARTESIAN_POINT('Origin',(-89.5,-64.5,51.5));
#15277=CARTESIAN_POINT('',(-89.5,-64.5,52.));
#15278=CARTESIAN_POINT('Origin',(-89.5,-64.5,51.5));
#15279=CARTESIAN_POINT('Origin',(-89.5,-64.5,51.5));
#15280=CARTESIAN_POINT('Origin',(89.5,18.545300072509,36.1978257430375));
#15281=CARTESIAN_POINT('',(89.5,19.045300072509,36.1978257430375));
#15282=CARTESIAN_POINT('Origin',(89.5,19.545300072509,36.1978257430375));
#15283=CARTESIAN_POINT('',(89.5,18.545300072509,35.6978257430375));
#15284=CARTESIAN_POINT('Origin',(89.5,18.545300072509,36.1978257430375));
#15285=CARTESIAN_POINT('Origin',(89.5,18.545300072509,35.1978257430375));
#15286=CARTESIAN_POINT('Origin',(-89.5,18.5453000725091,36.1978257430375));
#15287=CARTESIAN_POINT('',(-89.5,18.5453000725091,35.6978257430375));
#15288=CARTESIAN_POINT('Origin',(-89.5,18.5453000725091,35.1978257430375));
#15289=CARTESIAN_POINT('',(-89.5,19.0453000725091,36.1978257430375));
#15290=CARTESIAN_POINT('Origin',(-89.5,18.5453000725091,36.1978257430375));
#15291=CARTESIAN_POINT('Origin',(-89.5,19.5453000725091,36.1978257430375));
#15292=CARTESIAN_POINT('Origin',(-89.5,42.0226500362545,35.1978257430375));
#15293=CARTESIAN_POINT('',(-89.5,42.0226500362545,35.6978257430375));
#15294=CARTESIAN_POINT('Origin',(-90.,18.5453000725091,36.1978257430375));
#15295=CARTESIAN_POINT('',(-90.,18.5453000725091,35.6978257430375));
#15296=CARTESIAN_POINT('',(-90.,19.0453000725091,36.1978257430375));
#15297=CARTESIAN_POINT('Origin',(89.5,19.545300072509,47.1978257430375));
#15298=CARTESIAN_POINT('',(89.5,19.045300072509,47.1978257430375));
#15299=CARTESIAN_POINT('Origin',(89.5,19.545300072509,47.1978257430375));
#15300=CARTESIAN_POINT('',(89.5,19.545300072509,47.6978257430375));
#15301=CARTESIAN_POINT('Origin',(89.5,19.545300072509,47.1978257430375));
#15302=CARTESIAN_POINT('Origin',(89.5,19.545300072509,47.1978257430375));
#15303=CARTESIAN_POINT('Origin',(89.5,64.5,32.5));
#15304=CARTESIAN_POINT('',(89.5,65.,32.5));
#15305=CARTESIAN_POINT('Origin',(89.5,64.5,32.5));
#15306=CARTESIAN_POINT('',(89.5,64.5,32.));
#15307=CARTESIAN_POINT('Origin',(89.5,64.5,32.5));
#15308=CARTESIAN_POINT('Origin',(89.5,64.5,32.5));
#15309=CARTESIAN_POINT('Origin',(89.5,-32.5,32.5));
#15310=CARTESIAN_POINT('',(89.5,-32.5,32.));
#15311=CARTESIAN_POINT('Origin',(-89.5,19.5453000725091,47.1978257430375));
#15312=CARTESIAN_POINT('',(-89.5,19.5453000725091,47.6978257430375));
#15313=CARTESIAN_POINT('Origin',(-89.5,19.5453000725091,47.1978257430375));
#15314=CARTESIAN_POINT('',(-89.5,19.0453000725091,47.1978257430375));
#15315=CARTESIAN_POINT('Origin',(-89.5,19.5453000725091,47.1978257430375));
#15316=CARTESIAN_POINT('Origin',(-89.5,19.5453000725091,47.1978257430375));
#15317=CARTESIAN_POINT('Origin',(-89.5,19.5453000725091,39.8489128715187));
#15318=CARTESIAN_POINT('',(-89.5,19.0453000725091,39.8489128715187));
#15319=CARTESIAN_POINT('Origin',(-90.,19.5453000725091,47.1978257430375));
#15320=CARTESIAN_POINT('',(-90.,19.0453000725091,47.1978257430375));
#15321=CARTESIAN_POINT('',(-90.,19.5453000725091,47.6978257430375));
#15322=CARTESIAN_POINT('Origin',(-89.5,64.5,32.5));
#15323=CARTESIAN_POINT('',(-89.5,64.5,32.));
#15324=CARTESIAN_POINT('Origin',(-89.5,64.5,32.5));
#15325=CARTESIAN_POINT('Origin',(-89.5,64.5,32.5));
#15326=CARTESIAN_POINT('Origin',(45.,64.5,32.5));
#15327=CARTESIAN_POINT('',(45.,65.,32.5));
#15328=CARTESIAN_POINT('',(45.,64.5,32.));
#15329=CARTESIAN_POINT('Origin',(-89.5,32.5,32.5));
#15330=CARTESIAN_POINT('',(-89.5,32.5,32.));
#15331=CARTESIAN_POINT('Origin',(89.5,24.92755355845,48.1978257430375));
#15332=CARTESIAN_POINT('',(89.5,25.2811069490433,48.5513791336308));
#15333=CARTESIAN_POINT('Origin',(89.5,25.6346603396366,48.904932524224));
#15334=CARTESIAN_POINT('',(89.5,24.92755355845,47.6978257430375));
#15335=CARTESIAN_POINT('Origin',(89.5,24.92755355845,48.1978257430375));
#15336=CARTESIAN_POINT('Origin',(89.5,24.92755355845,47.1978257430375));
#15337=CARTESIAN_POINT('Origin',(89.5,64.5,51.5));
#15338=CARTESIAN_POINT('',(89.5,64.5,52.));
#15339=CARTESIAN_POINT('Origin',(89.5,64.5,51.5));
#15340=CARTESIAN_POINT('Origin',(89.5,64.5,51.5));
#15341=CARTESIAN_POINT('Origin',(89.5,64.5,32.));
#15342=CARTESIAN_POINT('',(89.5,65.,32.));
#15343=CARTESIAN_POINT('Origin',(-89.5,24.9275535584501,48.1978257430375));
#15344=CARTESIAN_POINT('',(-89.5,24.9275535584501,47.6978257430375));
#15345=CARTESIAN_POINT('Origin',(-89.5,24.9275535584501,47.1978257430375));
#15346=CARTESIAN_POINT('',(-89.5,25.2811069490433,48.5513791336308));
#15347=CARTESIAN_POINT('Origin',(-89.5,24.9275535584501,48.1978257430375));
#15348=CARTESIAN_POINT('Origin',(-89.5,25.6346603396366,48.904932524224));
#15349=CARTESIAN_POINT('Origin',(-89.5,64.5,51.5));
#15350=CARTESIAN_POINT('',(-89.5,64.5,52.));
#15351=CARTESIAN_POINT('Origin',(-89.5,64.5,51.5));
#15352=CARTESIAN_POINT('Origin',(-89.5,64.5,51.5));
#15353=CARTESIAN_POINT('Origin',(-89.5,64.5,51.5));
#15354=CARTESIAN_POINT('Origin',(-89.5,64.5,32.));
#15355=CARTESIAN_POINT('Origin',(89.5,23.0395928638606,51.5));
#15356=CARTESIAN_POINT('',(89.5,22.6860394732673,51.1464466094067));
#15357=CARTESIAN_POINT('',(89.5,23.0395928638606,52.));
#15358=CARTESIAN_POINT('Origin',(89.5,23.0395928638606,51.5));
#15359=CARTESIAN_POINT('Origin',(89.5,23.0395928638606,51.5));
#15360=CARTESIAN_POINT('Origin',(89.5,23.0395928638606,51.5));
#15361=CARTESIAN_POINT('Origin',(89.5,5.4779179525988,69.0616749112618));
#15362=CARTESIAN_POINT('',(89.5,5.12436456200553,68.7081215206685));
#15363=CARTESIAN_POINT('Origin',(89.5,-32.5,51.5));
#15364=CARTESIAN_POINT('',(89.5,-32.5,52.));
#15365=CARTESIAN_POINT('Origin',(-89.5,23.0395928638606,51.5));
#15366=CARTESIAN_POINT('',(-89.5,22.6860394732674,51.1464466094067));
#15367=CARTESIAN_POINT('Origin',(-89.5,23.0395928638606,51.5));
#15368=CARTESIAN_POINT('',(-89.5,23.0395928638606,52.));
#15369=CARTESIAN_POINT('Origin',(-89.5,23.0395928638606,51.5));
#15370=CARTESIAN_POINT('Origin',(-89.5,23.0395928638606,51.5));
#15371=CARTESIAN_POINT('Origin',(-45.,23.0395928638606,51.5));
#15372=CARTESIAN_POINT('',(-45.,23.0395928638606,52.));
#15373=CARTESIAN_POINT('',(-45.,22.6860394732673,51.1464466094067));
#15374=CARTESIAN_POINT('Origin',(-89.5,32.5,51.5));
#15375=CARTESIAN_POINT('',(-89.5,32.5,52.));
#15376=CARTESIAN_POINT('Origin',(-89.5,37.9779179525988,36.5616749112618));
#15377=CARTESIAN_POINT('',(-89.5,37.6243645620056,36.2081215206685));
#15378=CARTESIAN_POINT('Origin',(45.,64.5,51.5));
#15379=CARTESIAN_POINT('',(45.,64.5,52.));
#15380=CARTESIAN_POINT('Origin',(-89.5,45.5673301698183,47.1978257430375));
#15381=CARTESIAN_POINT('',(-89.5,45.5673301698183,47.6978257430375));
#15382=CARTESIAN_POINT('Origin',(-90.,24.9275535584501,48.1978257430375));
#15383=CARTESIAN_POINT('',(-90.,24.9275535584501,47.6978257430375));
#15384=CARTESIAN_POINT('',(-90.,25.2811069490433,48.5513791336308));
#15385=CARTESIAN_POINT('Origin',(89.5,-19.4326698301817,47.1978257430375));
#15386=CARTESIAN_POINT('',(89.5,-19.4326698301817,47.6978257430375));
#15387=CARTESIAN_POINT('Origin',(89.5,19.545300072509,39.8489128715187));
#15388=CARTESIAN_POINT('',(89.5,19.045300072509,39.8489128715187));
#15389=CARTESIAN_POINT('Origin',(89.5,-22.9773499637455,35.1978257430375));
#15390=CARTESIAN_POINT('',(89.5,-22.9773499637455,35.6978257430375));
#15391=CARTESIAN_POINT('Origin',(-45.,-64.5,51.5));
#15392=CARTESIAN_POINT('',(-45.,-64.5,52.));
#15393=CARTESIAN_POINT('Origin',(-89.5,32.5,51.5));
#15394=CARTESIAN_POINT('',(-89.5,32.5,52.));
#15395=CARTESIAN_POINT('Origin',(89.5,-32.5,51.5));
#15396=CARTESIAN_POINT('',(89.5,-32.5,52.));
#15397=CARTESIAN_POINT('Origin',(89.5,-22.0741207385024,33.8489128715187));
#15398=CARTESIAN_POINT('',(89.5,-21.5741207385024,33.8489128715187));
#15399=CARTESIAN_POINT('Origin',(89.5,-43.2870603692512,47.1978257430375));
#15400=CARTESIAN_POINT('',(89.5,-43.2870603692512,47.6978257430375));
#15401=CARTESIAN_POINT('Origin',(-90.,-44.3272645584124,48.1978257430375));
#15402=CARTESIAN_POINT('',(-90.,-44.8272645584124,48.1978257430375));
#15403=CARTESIAN_POINT('',(-90.,-44.3272645584124,47.6978257430375));
#15404=CARTESIAN_POINT('Origin',(0.,0.,32.));
#15405=CARTESIAN_POINT('Origin',(-90.,-44.8272645584124,47.6978257430375));
#15406=CARTESIAN_POINT('Origin',(-90.,-21.5741207385023,47.6978257430375));
#15407=CARTESIAN_POINT('Origin',(-90.,-21.5741207385023,35.6978257430375));
#15408=CARTESIAN_POINT('Origin',(-90.,19.0453000725091,35.6978257430375));
#15409=CARTESIAN_POINT('Origin',(-90.,19.0453000725091,47.6978257430375));
#15410=CARTESIAN_POINT('Origin',(-90.,26.1346603396366,47.6978257430375));
#15411=CARTESIAN_POINT('Origin',(90.,65.,32.));
#15412=CARTESIAN_POINT('Origin',(-90.,21.8324860826741,52.));
#15413=CARTESIAN_POINT('Origin',(0.,0.,52.));
#15414=CARTESIAN_POINT('Origin',(0.,0.,52.));
#15415=CARTESIAN_POINT('',(0.,0.,0.));
#15416=CARTESIAN_POINT('Origin',(-69.9040264336917,64.8,3.08953555269655));
#15417=CARTESIAN_POINT('',(-104.475451921837,64.8,2.78953555269655));
#15418=CARTESIAN_POINT('',(-104.475451921837,64.5,3.08953555269655));
#15419=CARTESIAN_POINT('Origin',(-104.475451921837,64.8,3.08953555269655));
#15420=CARTESIAN_POINT('',(-77.8080528673835,64.8,2.78953555269655));
#15421=CARTESIAN_POINT('',(-69.9040264336917,64.8,2.78953555269655));
#15422=CARTESIAN_POINT('',(-77.8080528673835,64.5,3.08953555269655));
#15423=CARTESIAN_POINT('Origin',(-77.8080528673835,64.8,3.08953555269655));
#15424=CARTESIAN_POINT('',(-69.9040264336917,64.5,3.08953555269655));
#15425=CARTESIAN_POINT('Origin',(-77.8080528673835,60.,3.08953555269655));
#15426=CARTESIAN_POINT('',(-77.8080528673835,55.5,3.08953555269655));
#15427=CARTESIAN_POINT('',(-77.8080528673835,55.2,2.78953555269655));
#15428=CARTESIAN_POINT('Origin',(-77.8080528673835,55.2,3.08953555269655));
#15429=CARTESIAN_POINT('Origin',(-77.8080528673835,60.,3.08953555269655));
#15430=CARTESIAN_POINT('Origin',(-77.8080528673835,60.,2.78953555269655));
#15431=CARTESIAN_POINT('Origin',(-83.2377259609183,55.2,3.08953555269655));
#15432=CARTESIAN_POINT('',(-104.475451921837,55.5,3.08953555269655));
#15433=CARTESIAN_POINT('',(-104.475451921837,55.2,2.78953555269655));
#15434=CARTESIAN_POINT('Origin',(-104.475451921837,55.2,3.08953555269655));
#15435=CARTESIAN_POINT('',(-83.2377259609183,55.5,3.08953555269655));
#15436=CARTESIAN_POINT('',(-83.2377259609183,55.2,2.78953555269655));
#15437=CARTESIAN_POINT('Origin',(-104.475451921837,60.,3.08953555269655));
#15438=CARTESIAN_POINT('Origin',(-104.475451921837,60.,3.08953555269655));
#15439=CARTESIAN_POINT('Origin',(-104.475451921837,60.,2.78953555269655));
#15440=CARTESIAN_POINT('Origin',(-77.8080528673835,60.,10.7895355526966));
#15441=CARTESIAN_POINT('',(-77.8080528673835,55.5,10.4895355526966));
#15442=CARTESIAN_POINT('',(-77.8080528673835,55.5,10.7895355526966));
#15443=CARTESIAN_POINT('',(-77.8080528673835,64.5,10.4895355526966));
#15444=CARTESIAN_POINT('Origin',(-77.8080528673835,60.,10.4895355526966));
#15445=CARTESIAN_POINT('',(-77.8080528673835,64.5,10.7895355526966));
#15446=CARTESIAN_POINT('Origin',(-77.8080528673835,64.5,10.7895355526966));
#15447=CARTESIAN_POINT('',(-104.475451921837,64.5,10.4895355526966));
#15448=CARTESIAN_POINT('',(-94.9040264336917,64.5,10.4895355526966));
#15449=CARTESIAN_POINT('',(-104.475451921837,64.5,10.7895355526966));
#15450=CARTESIAN_POINT('Origin',(-62.,70.,2.78953555269655));
#15451=CARTESIAN_POINT('',(-109.7,69.7,2.78953555269655));
#15452=CARTESIAN_POINT('',(-62.7242640687119,69.7,2.78953555269655));
#15453=CARTESIAN_POINT('',(-74.5,69.7,2.78953555269655));
#15454=CARTESIAN_POINT('',(-62.7242640687119,50.3,2.78953555269655));
#15455=CARTESIAN_POINT('',(-62.7242640687119,70.,2.78953555269655));
#15456=CARTESIAN_POINT('',(-109.7,50.3,2.78953555269655));
#15457=CARTESIAN_POINT('',(-74.5,50.3,2.78953555269655));
#15458=CARTESIAN_POINT('',(-109.7,70.,2.78953555269655));
#15459=CARTESIAN_POINT('Origin',(-109.7,50.3,2.48953555269655));
#15460=CARTESIAN_POINT('',(-109.7,50.,3.08953555269655));
#15461=CARTESIAN_POINT('Origin',(-109.7,50.3,3.08953555269655));
#15462=CARTESIAN_POINT('',(-110.3,50.,2.48953555269655));
#15463=CARTESIAN_POINT('Origin',(-109.7,50.,2.48953555269655));
#15464=CARTESIAN_POINT('',(-110.,50.3,2.48953555269655));
#15465=CARTESIAN_POINT('Origin',(-110.3,50.3,2.48953555269655));
#15466=CARTESIAN_POINT('Origin',(-109.7,50.3,2.48953555269655));
#15467=CARTESIAN_POINT('Origin',(-111.7,50.3,0.3));
#15468=CARTESIAN_POINT('',(-111.7,50.3,0.));
#15469=CARTESIAN_POINT('',(-111.7,50.,0.3));
#15470=CARTESIAN_POINT('Origin',(-111.7,50.3,0.3));
#15471=CARTESIAN_POINT('',(-112.,50.3,0.3));
#15472=CARTESIAN_POINT('Origin',(-111.7,50.3,0.3));
#15473=CARTESIAN_POINT('Origin',(-111.7,50.3,0.3));
#15474=CARTESIAN_POINT('Origin',(-109.7,69.7,2.48953555269655));
#15475=CARTESIAN_POINT('',(-109.7,70.,3.08953555269655));
#15476=CARTESIAN_POINT('',(-110.3,70.,2.48953555269655));
#15477=CARTESIAN_POINT('Origin',(-109.7,70.,2.48953555269655));
#15478=CARTESIAN_POINT('Origin',(-109.7,69.7,3.08953555269655));
#15479=CARTESIAN_POINT('',(-110.,69.7,2.48953555269655));
#15480=CARTESIAN_POINT('Origin',(-109.7,69.7,2.48953555269655));
#15481=CARTESIAN_POINT('Origin',(-110.3,69.7,2.48953555269655));
#15482=CARTESIAN_POINT('Origin',(-110.3,69.7,4.09215166452241));
#15483=CARTESIAN_POINT('',(-110.,69.7,0.));
#15484=CARTESIAN_POINT('',(-110.,69.7,4.09215166452241));
#15485=CARTESIAN_POINT('',(-110.3,70.,0.3));
#15486=CARTESIAN_POINT('Origin',(-110.3,69.7,0.3));
#15487=CARTESIAN_POINT('',(-110.3,70.,4.09215166452241));
#15488=CARTESIAN_POINT('Origin',(-62.7242640687119,50.3,3.08953555269655));
#15489=CARTESIAN_POINT('',(-62.512132034356,50.3,3.30166758705252));
#15490=CARTESIAN_POINT('',(-62.7242640687119,50.,3.08953555269655));
#15491=CARTESIAN_POINT('Origin',(-62.7242640687119,50.3,3.08953555269656));
#15492=CARTESIAN_POINT('Origin',(-62.7242640687119,50.3,3.08953555269655));
#15493=CARTESIAN_POINT('Origin',(-62.7242640687119,50.3,3.08953555269655));
#15494=CARTESIAN_POINT('Origin',(-111.7,69.7,0.3));
#15495=CARTESIAN_POINT('',(-111.7,69.7,0.));
#15496=CARTESIAN_POINT('',(-112.,69.7,0.3));
#15497=CARTESIAN_POINT('Origin',(-111.7,69.7,0.3));
#15498=CARTESIAN_POINT('',(-111.7,70.,0.3));
#15499=CARTESIAN_POINT('Origin',(-111.7,69.7,0.3));
#15500=CARTESIAN_POINT('Origin',(-111.7,69.7,0.3));
#15501=CARTESIAN_POINT('Origin',(-98.5,69.7,0.3));
#15502=CARTESIAN_POINT('',(-98.5,70.,0.3));
#15503=CARTESIAN_POINT('',(-98.5,69.7,0.));
#15504=CARTESIAN_POINT('Origin',(-111.7,50.3,10.4895355526966));
#15505=CARTESIAN_POINT('',(-112.,50.3,10.4895355526966));
#15506=CARTESIAN_POINT('',(-111.7,50.,10.4895355526966));
#15507=CARTESIAN_POINT('Origin',(-111.7,50.3,10.4895355526966));
#15508=CARTESIAN_POINT('',(-111.7,50.3,10.7895355526966));
#15509=CARTESIAN_POINT('Origin',(-111.7,50.3,10.4895355526966));
#15510=CARTESIAN_POINT('Origin',(-111.7,50.3,10.4895355526966));
#15511=CARTESIAN_POINT('Origin',(-62.7242640687119,69.7,3.08953555269655));
#15512=CARTESIAN_POINT('',(-62.512132034356,69.7,3.30166758705252));
#15513=CARTESIAN_POINT('Origin',(-62.7242640687119,69.7,3.08953555269655));
#15514=CARTESIAN_POINT('',(-62.7242640687119,70.,3.08953555269655));
#15515=CARTESIAN_POINT('Origin',(-62.7242640687119,69.7,3.08953555269655));
#15516=CARTESIAN_POINT('Origin',(-62.7242640687119,69.7,3.08953555269655));
#15517=CARTESIAN_POINT('Origin',(-70.1242640687119,50.3,10.4895355526966));
#15518=CARTESIAN_POINT('',(-70.1242640687119,50.3,10.7895355526966));
#15519=CARTESIAN_POINT('',(-70.1242640687119,50.,10.4895355526966));
#15520=CARTESIAN_POINT('Origin',(-70.1242640687119,50.3,10.4895355526966));
#15521=CARTESIAN_POINT('',(-69.9121320343559,50.3,10.7016675870525));
#15522=CARTESIAN_POINT('Origin',(-70.1242640687119,50.3,10.4895355526966));
#15523=CARTESIAN_POINT('Origin',(-70.1242640687119,50.3,10.4895355526966));
#15524=CARTESIAN_POINT('Origin',(-111.7,69.7,10.4895355526966));
#15525=CARTESIAN_POINT('',(-112.,69.7,10.4895355526966));
#15526=CARTESIAN_POINT('',(-111.7,69.7,10.7895355526966));
#15527=CARTESIAN_POINT('Origin',(-111.7,69.7,10.4895355526966));
#15528=CARTESIAN_POINT('',(-111.7,70.,10.4895355526966));
#15529=CARTESIAN_POINT('Origin',(-111.7,69.7,10.4895355526966));
#15530=CARTESIAN_POINT('Origin',(-111.7,69.7,10.4895355526966));
#15531=CARTESIAN_POINT('Origin',(-111.7,69.7,2.69738388817414));
#15532=CARTESIAN_POINT('',(-111.7,70.,2.69738388817414));
#15533=CARTESIAN_POINT('',(-112.,69.7,2.69738388817414));
#15534=CARTESIAN_POINT('Origin',(-70.1242640687119,69.7,10.4895355526966));
#15535=CARTESIAN_POINT('',(-70.1242640687119,69.7,10.7895355526966));
#15536=CARTESIAN_POINT('',(-69.9121320343559,69.7,10.7016675870525));
#15537=CARTESIAN_POINT('Origin',(-70.1242640687119,69.7,10.4895355526966));
#15538=CARTESIAN_POINT('',(-70.1242640687119,70.,10.4895355526966));
#15539=CARTESIAN_POINT('Origin',(-70.1242640687119,69.7,10.4895355526966));
#15540=CARTESIAN_POINT('Origin',(-70.1242640687119,69.7,10.4895355526966));
#15541=CARTESIAN_POINT('Origin',(-99.5,69.7,10.4895355526966));
#15542=CARTESIAN_POINT('',(-99.5,69.7,10.7895355526966));
#15543=CARTESIAN_POINT('',(-99.5,70.,10.4895355526966));
#15544=CARTESIAN_POINT('Origin',(-73.1134400902689,69.7,13.4787115742535));
#15545=CARTESIAN_POINT('',(-72.9013080559129,69.7,13.6908436086095));
#15546=CARTESIAN_POINT('',(-73.1134400902689,70.,13.4787115742535));
#15547=CARTESIAN_POINT('Origin',(-70.1242640687119,70.,10.4895355526966));
#15548=CARTESIAN_POINT('',(-69.9121320343559,70.,10.7016675870525));
#15549=CARTESIAN_POINT('',(-70.1242640687119,70.,10.7895355526966));
#15550=CARTESIAN_POINT('Origin',(-111.7,70.,10.4895355526966));
#15551=CARTESIAN_POINT('',(-111.7,70.,10.7895355526966));
#15552=CARTESIAN_POINT('',(-112.,70.,10.4895355526966));
#15553=CARTESIAN_POINT('Origin',(-73.1134400902689,50.3,13.4787115742535));
#15554=CARTESIAN_POINT('',(-72.9013080559129,50.3,13.6908436086095));
#15555=CARTESIAN_POINT('',(-73.1134400902689,50.,13.4787115742535));
#15556=CARTESIAN_POINT('Origin',(-99.5,50.3,10.4895355526966));
#15557=CARTESIAN_POINT('',(-99.5,50.3,10.7895355526966));
#15558=CARTESIAN_POINT('',(-99.5,50.,10.4895355526966));
#15559=CARTESIAN_POINT('Origin',(-74.5,69.7,3.08953555269655));
#15560=CARTESIAN_POINT('',(-74.5,70.,3.08953555269655));
#15561=CARTESIAN_POINT('Origin',(-62.7242640687119,70.,3.08953555269655));
#15562=CARTESIAN_POINT('',(-62.512132034356,70.,3.30166758705252));
#15563=CARTESIAN_POINT('Origin',(-111.7,50.3,2.69738388817414));
#15564=CARTESIAN_POINT('',(-112.,50.3,2.69738388817414));
#15565=CARTESIAN_POINT('',(-111.7,50.,2.69738388817414));
#15566=CARTESIAN_POINT('Origin',(-111.7,70.,0.3));
#15567=CARTESIAN_POINT('',(-112.,70.,0.3));
#15568=CARTESIAN_POINT('',(-111.7,70.,0.));
#15569=CARTESIAN_POINT('Origin',(-74.5,50.3,3.08953555269655));
#15570=CARTESIAN_POINT('',(-74.5,50.,3.08953555269655));
#15571=CARTESIAN_POINT('Origin',(-109.7,70.,2.48953555269655));
#15572=CARTESIAN_POINT('',(-110.,70.,2.48953555269655));
#15573=CARTESIAN_POINT('Origin',(-98.5,50.3,0.3));
#15574=CARTESIAN_POINT('',(-110.,50.3,0.));
#15575=CARTESIAN_POINT('',(-98.5,50.3,0.));
#15576=CARTESIAN_POINT('',(-110.3,50.,0.3));
#15577=CARTESIAN_POINT('Origin',(-110.3,50.3,0.3));
#15578=CARTESIAN_POINT('',(-98.5,50.,0.3));
#15579=CARTESIAN_POINT('Origin',(-110.3,50.3,4.09215166452241));
#15580=CARTESIAN_POINT('',(-110.3,50.,4.09215166452241));
#15581=CARTESIAN_POINT('',(-110.,50.3,4.09215166452241));
#15582=CARTESIAN_POINT('Origin',(-110.,70.,2.78953555269655));
#15583=CARTESIAN_POINT('',(-110.,70.,0.));
#15584=CARTESIAN_POINT('Origin',(-87.,70.,5.39476777634828));
#15585=CARTESIAN_POINT('Origin',(-112.,70.,0.));
#15586=CARTESIAN_POINT('Origin',(-112.,70.,10.7895355526966));
#15587=CARTESIAN_POINT('',(-104.475451921837,64.8,10.7895355526966));
#15588=CARTESIAN_POINT('',(-77.8080528673835,64.8,10.7895355526966));
#15589=CARTESIAN_POINT('',(-94.9040264336917,64.8,10.7895355526966));
#15590=CARTESIAN_POINT('',(-77.8080528673835,55.2,10.7895355526966));
#15591=CARTESIAN_POINT('Origin',(-77.8080528673835,60.,10.7895355526966));
#15592=CARTESIAN_POINT('',(-104.475451921837,55.2,10.7895355526966));
#15593=CARTESIAN_POINT('',(-108.237725960918,55.2,10.7895355526966));
#15594=CARTESIAN_POINT('Origin',(-104.475451921837,60.,10.7895355526966));
#15595=CARTESIAN_POINT('Origin',(-70.,70.,10.7895355526965));
#15596=CARTESIAN_POINT('Origin',(-87.,50.,5.39476777634828));
#15597=CARTESIAN_POINT('Origin',(-94.9040264336917,64.8,10.4895355526966));
#15598=CARTESIAN_POINT('Origin',(-77.8080528673835,64.8,10.4895355526966));
#15599=CARTESIAN_POINT('Origin',(-104.475451921837,64.8,10.4895355526966));
#15600=CARTESIAN_POINT('Origin',(-104.475451921837,60.,10.4895355526966));
#15601=CARTESIAN_POINT('',(-104.475451921837,55.5,10.4895355526966));
#15602=CARTESIAN_POINT('Origin',(-104.475451921837,55.2,10.4895355526966));
#15603=CARTESIAN_POINT('Origin',(-104.475451921837,60.,10.4895355526966));
#15604=CARTESIAN_POINT('Origin',(-108.237725960918,55.2,10.4895355526966));
#15605=CARTESIAN_POINT('Origin',(-77.8080528673835,55.2,10.4895355526966));
#15606=CARTESIAN_POINT('',(-108.237725960918,55.5,10.4895355526966));
#15607=CARTESIAN_POINT('Origin',(-77.8080528673835,60.,10.4895355526966));
#15608=CARTESIAN_POINT('Origin',(-104.475451921837,60.,10.7895355526966));
#15609=CARTESIAN_POINT('',(-104.475451921837,55.5,10.7895355526966));
#15610=CARTESIAN_POINT('Origin',(-104.475451921837,55.5,10.7895355526966));
#15611=CARTESIAN_POINT('Origin',(-110.,70.,0.));
#15612=CARTESIAN_POINT('',(0.,0.,0.));
#15613=CARTESIAN_POINT('Origin',(-71.2994615223724,45.9821613702938,64.));
#15614=CARTESIAN_POINT('',(-58.7994615223724,45.9821613702938,64.));
#15615=CARTESIAN_POINT('Origin',(-71.2994615223724,45.9821613702938,64.));
#15616=CARTESIAN_POINT('',(-58.7994615223724,45.9821613702938,52.));
#15617=CARTESIAN_POINT('',(-58.7994615223724,45.9821613702938,64.));
#15618=CARTESIAN_POINT('Origin',(-71.2994615223724,45.9821613702938,52.));
#15619=CARTESIAN_POINT('Origin',(-71.2994615223724,-45.9821613702938,64.));
#15620=CARTESIAN_POINT('',(-58.7994615223724,-45.9821613702938,64.));
#15621=CARTESIAN_POINT('Origin',(-71.2994615223724,-45.9821613702938,64.));
#15622=CARTESIAN_POINT('',(-58.7994615223724,-45.9821613702938,52.));
#15623=CARTESIAN_POINT('',(-58.7994615223724,-45.9821613702938,64.));
#15624=CARTESIAN_POINT('',(-83.7822941402435,-45.3272645584124,52.));
#15625=CARTESIAN_POINT('Origin',(-71.2994615223724,-45.9821613702938,52.));
#15626=CARTESIAN_POINT('',(-83.745995712817,-44.8272645584124,51.5));
#15627=CARTESIAN_POINT('Ctrl Pts',(-83.745995712817,-44.8272645584124,51.5));
#15628=CARTESIAN_POINT('Ctrl Pts',(-83.745995712817,-44.8272645584124,51.5628289407498));
#15629=CARTESIAN_POINT('Ctrl Pts',(-83.747181725005,-44.83983109791,51.6298216562663));
#15630=CARTESIAN_POINT('Ctrl Pts',(-83.7517608175057,-44.8908782000976,
51.7530059059081));
#15631=CARTESIAN_POINT('Ctrl Pts',(-83.7551262217237,-44.9293569823107,
51.8091992050848));
#15632=CARTESIAN_POINT('Ctrl Pts',(-83.762309793067,-45.0181089553366,51.8979511781107));
#15633=CARTESIAN_POINT('Ctrl Pts',(-83.7666038574713,-45.0743219277052,
51.936421701237));
#15634=CARTESIAN_POINT('Ctrl Pts',(-83.7749619719384,-45.1974964800649,
51.9874465324277));
#15635=CARTESIAN_POINT('Ctrl Pts',(-83.7789991865087,-45.264460227701,52.));
#15636=CARTESIAN_POINT('Ctrl Pts',(-83.7822941402435,-45.3272645584124,
52.));
#15637=CARTESIAN_POINT('',(-83.745995712817,-44.8272645584124,48.1978257430375));
#15638=CARTESIAN_POINT('',(-83.745995712817,-44.8272645584124,64.));
#15639=CARTESIAN_POINT('',(-83.6894299057874,-44.3272645584124,47.6978257430375));
#15640=CARTESIAN_POINT('Ctrl Pts',(-83.6894299057874,-44.3272645584124,
47.6978257430375));
#15641=CARTESIAN_POINT('Ctrl Pts',(-83.6977893835036,-44.3898507353037,
47.6978257430375));
#15642=CARTESIAN_POINT('Ctrl Pts',(-83.7061896428019,-44.4567282803348,
47.7102969796753));
#15643=CARTESIAN_POINT('Ctrl Pts',(-83.7207197517911,-44.5799514130651,
47.7612544377797));
#15644=CARTESIAN_POINT('Ctrl Pts',(-83.7268763359328,-44.636291625979,47.7997460294175));
#15645=CARTESIAN_POINT('Ctrl Pts',(-83.7361763124954,-44.7251367458781,
47.8885911493166));
#15646=CARTESIAN_POINT('Ctrl Pts',(-83.7399528718684,-44.7636241839714,
47.9447717029639));
#15647=CARTESIAN_POINT('Ctrl Pts',(-83.7448488457163,-44.8146887744293,
48.0679654140368));
#15648=CARTESIAN_POINT('Ctrl Pts',(-83.745995712817,-44.8272645584124,48.1349780461073));
#15649=CARTESIAN_POINT('Ctrl Pts',(-83.745995712817,-44.8272645584124,48.1978257430375));
#15650=CARTESIAN_POINT('',(-58.9094931389573,-44.3272645584124,47.6978257430375));
#15651=CARTESIAN_POINT('Origin',(-71.2994615223724,-45.9821613702938,47.6978257430375));
#15652=CARTESIAN_POINT('',(-58.8529273319278,-44.8272645584124,48.1978257430375));
#15653=CARTESIAN_POINT('Ctrl Pts',(-58.8529273319278,-44.8272645584124,
48.1978257430375));
#15654=CARTESIAN_POINT('Ctrl Pts',(-58.8529273319278,-44.8272645584124,
48.1349780461073));
#15655=CARTESIAN_POINT('Ctrl Pts',(-58.8540741990285,-44.8146887744293,
48.0679654140368));
#15656=CARTESIAN_POINT('Ctrl Pts',(-58.8589701728764,-44.7636241839714,
47.9447717029639));
#15657=CARTESIAN_POINT('Ctrl Pts',(-58.8627467322493,-44.7251367458781,
47.8885911493166));
#15658=CARTESIAN_POINT('Ctrl Pts',(-58.872046708812,-44.636291625979,47.7997460294175));
#15659=CARTESIAN_POINT('Ctrl Pts',(-58.8782032929536,-44.5799514130651,
47.7612544377797));
#15660=CARTESIAN_POINT('Ctrl Pts',(-58.8927334019429,-44.4567282803348,
47.7102969796753));
#15661=CARTESIAN_POINT('Ctrl Pts',(-58.9011336612412,-44.3898507353037,
47.6978257430375));
#15662=CARTESIAN_POINT('Ctrl Pts',(-58.9094931389573,-44.3272645584124,
47.6978257430375));
#15663=CARTESIAN_POINT('',(-58.8529273319278,-44.8272645584124,51.5));
#15664=CARTESIAN_POINT('',(-58.8529273319278,-44.8272645584124,64.));
#15665=CARTESIAN_POINT('',(-58.8166289045013,-45.3272645584124,52.));
#15666=CARTESIAN_POINT('Ctrl Pts',(-58.8166289045013,-45.3272645584124,
52.));
#15667=CARTESIAN_POINT('Ctrl Pts',(-58.8199238582361,-45.264460227701,52.));
#15668=CARTESIAN_POINT('Ctrl Pts',(-58.8239610728064,-45.1974964800649,
51.9874465324277));
#15669=CARTESIAN_POINT('Ctrl Pts',(-58.8323191872735,-45.0743219277052,
51.9364217012371));
#15670=CARTESIAN_POINT('Ctrl Pts',(-58.8366132516778,-45.0181089553366,
51.8979511781107));
#15671=CARTESIAN_POINT('Ctrl Pts',(-58.8437968230211,-44.9293569823107,
51.8091992050848));
#15672=CARTESIAN_POINT('Ctrl Pts',(-58.847162227239,-44.8908782000976,51.7530059059082));
#15673=CARTESIAN_POINT('Ctrl Pts',(-58.8517413197398,-44.83983109791,51.6298216562663));
#15674=CARTESIAN_POINT('Ctrl Pts',(-58.8529273319278,-44.8272645584124,
51.5628289407498));
#15675=CARTESIAN_POINT('Ctrl Pts',(-58.8529273319278,-44.8272645584124,
51.5));
#15676=CARTESIAN_POINT('Origin',(-71.2994615223724,-45.9821613702938,52.));
#15677=CARTESIAN_POINT('Origin',(-90.,-21.5741207385023,47.6978257430375));
#15678=CARTESIAN_POINT('',(-89.5,-44.3272645584124,47.6978257430375));
#15679=CARTESIAN_POINT('',(-90.,-44.3272645584124,47.6978257430375));
#15680=CARTESIAN_POINT('',(-89.5,-22.0741207385023,47.6978257430375));
#15681=CARTESIAN_POINT('',(-89.5,21.7129396307488,47.6978257430375));
#15682=CARTESIAN_POINT('',(-59.5720117555674,-22.0741207385024,47.6978257430375));
#15683=CARTESIAN_POINT('',(-90.,-22.0741207385023,47.6978257430375));
#15684=CARTESIAN_POINT('',(-49.8290651996878,-22.0741207385024,47.6978257430375));
#15685=CARTESIAN_POINT('Origin',(-54.7005384776276,-20.9477335482704,47.6978257430375));
#15686=CARTESIAN_POINT('',(-17.5720117555674,-22.0741207385024,47.6978257430375));
#15687=CARTESIAN_POINT('',(-90.,-22.0741207385023,47.6978257430375));
#15688=CARTESIAN_POINT('',(-7.82906519968783,-22.0741207385024,47.6978257430375));
#15689=CARTESIAN_POINT('Origin',(-12.7005384776276,-20.9477335482704,47.6978257430375));
#15690=CARTESIAN_POINT('',(24.4279882444326,-22.0741207385024,47.6978257430375));
#15691=CARTESIAN_POINT('',(-90.,-22.0741207385023,47.6978257430375));
#15692=CARTESIAN_POINT('',(34.1709348003122,-22.0741207385024,47.6978257430375));
#15693=CARTESIAN_POINT('Origin',(29.2994615223724,-20.9477335482704,47.6978257430375));
#15694=CARTESIAN_POINT('',(66.4279882444326,-22.0741207385024,47.6978257430375));
#15695=CARTESIAN_POINT('',(-90.,-22.0741207385023,47.6978257430375));
#15696=CARTESIAN_POINT('',(76.1709348003122,-22.0741207385024,47.6978257430375));
#15697=CARTESIAN_POINT('Origin',(71.2994615223724,-20.9477335482704,47.6978257430375));
#15698=CARTESIAN_POINT('',(89.5,-22.0741207385024,47.6978257430375));
#15699=CARTESIAN_POINT('',(-90.,-22.0741207385023,47.6978257430375));
#15700=CARTESIAN_POINT('',(89.5,-44.3272645584125,47.6978257430375));
#15701=CARTESIAN_POINT('',(89.5,-43.2870603692512,47.6978257430375));
#15702=CARTESIAN_POINT('',(83.6894299057875,-44.3272645584125,47.6978257430375));
#15703=CARTESIAN_POINT('',(-90.,-44.3272645584124,47.6978257430375));
#15704=CARTESIAN_POINT('',(58.9094931389573,-44.3272645584125,47.6978257430375));
#15705=CARTESIAN_POINT('Origin',(71.2994615223724,-45.9821613702938,47.6978257430375));
#15706=CARTESIAN_POINT('',(54.6969417294651,-44.3272645584125,47.6978257430375));
#15707=CARTESIAN_POINT('',(-90.,-44.3272645584124,47.6978257430375));
#15708=CARTESIAN_POINT('',(55.2994615223724,-41.9477335482704,47.6978257430375));
#15709=CARTESIAN_POINT('Origin',(50.2994615223724,-41.9477335482704,47.6978257430375));
#15710=CARTESIAN_POINT('',(45.9019813152797,-44.3272645584125,47.6978257430375));
#15711=CARTESIAN_POINT('Origin',(50.2994615223724,-41.9477335482704,47.6978257430375));
#15712=CARTESIAN_POINT('',(12.6969417294651,-44.3272645584125,47.6978257430375));
#15713=CARTESIAN_POINT('',(-90.,-44.3272645584124,47.6978257430375));
#15714=CARTESIAN_POINT('',(13.2994615223724,-41.9477335482704,47.6978257430375));
#15715=CARTESIAN_POINT('Origin',(8.29946152237238,-41.9477335482704,47.6978257430375));
#15716=CARTESIAN_POINT('',(3.90198131527965,-44.3272645584125,47.6978257430375));
#15717=CARTESIAN_POINT('Origin',(8.29946152237238,-41.9477335482704,47.6978257430375));
#15718=CARTESIAN_POINT('',(-29.3030582705349,-44.3272645584125,47.6978257430375));
#15719=CARTESIAN_POINT('',(-90.,-44.3272645584124,47.6978257430375));
#15720=CARTESIAN_POINT('',(-28.7005384776276,-41.9477335482704,47.6978257430375));
#15721=CARTESIAN_POINT('Origin',(-33.7005384776276,-41.9477335482704,47.6978257430375));
#15722=CARTESIAN_POINT('',(-38.0980186847204,-44.3272645584125,47.6978257430375));
#15723=CARTESIAN_POINT('Origin',(-33.7005384776276,-41.9477335482704,47.6978257430375));
#15724=CARTESIAN_POINT('',(-90.,-44.3272645584124,47.6978257430375));
#15725=CARTESIAN_POINT('Origin',(-90.,-44.3272645584124,48.1978257430375));
#15726=CARTESIAN_POINT('',(-89.5,-44.8272645584124,48.1978257430375));
#15727=CARTESIAN_POINT('',(-90.,-44.8272645584124,48.1978257430375));
#15728=CARTESIAN_POINT('Origin',(-89.5,-44.3272645584124,48.1978257430375));
#15729=CARTESIAN_POINT('Origin',(-90.,-44.8272645584124,47.6978257430375));
#15730=CARTESIAN_POINT('',(-89.5,-44.8272645584124,51.5));
#15731=CARTESIAN_POINT('',(-45.,-44.8272645584124,51.5));
#15732=CARTESIAN_POINT('',(-89.5,-44.8272645584124,49.8489128715187));
#15733=CARTESIAN_POINT('Origin',(-45.,-45.3272645584124,51.5));
#15734=CARTESIAN_POINT('',(-89.5,-45.3272645584124,52.));
#15735=CARTESIAN_POINT('',(-45.,-45.3272645584124,52.));
#15736=CARTESIAN_POINT('Origin',(-89.5,-45.3272645584124,51.5));
#15737=CARTESIAN_POINT('Origin',(50.2994615223724,-41.9477335482704,64.));
#15738=CARTESIAN_POINT('',(55.2994615223724,-41.9477335482704,64.));
#15739=CARTESIAN_POINT('Origin',(50.2994615223724,-41.9477335482704,64.));
#15740=CARTESIAN_POINT('',(55.2994615223724,-41.9477335482704,64.));
#15741=CARTESIAN_POINT('',(54.3870404098839,-44.8272645584125,48.1978257430375));
#15742=CARTESIAN_POINT('Ctrl Pts',(54.3870404098839,-44.8272645584125,48.1978257430375));
#15743=CARTESIAN_POINT('Ctrl Pts',(54.3870404098839,-44.8272645584125,48.1321584122493));
#15744=CARTESIAN_POINT('Ctrl Pts',(54.3967984405243,-44.8135380049882,48.0636994127672));
#15745=CARTESIAN_POINT('Ctrl Pts',(54.4328078861395,-44.7613527165995,47.9408836439009));
#15746=CARTESIAN_POINT('Ctrl Pts',(54.4588553021428,-44.7229773515989,47.8864317550374));
#15747=CARTESIAN_POINT('Ctrl Pts',(54.516109620418,-44.6352673224994,47.7987217259379));
#15748=CARTESIAN_POINT('Ctrl Pts',(54.5518807965474,-44.5787128115292,47.7605853033887));
#15749=CARTESIAN_POINT('Ctrl Pts',(54.6254379450942,-44.4559300231492,47.710126421675));
#15750=CARTESIAN_POINT('Ctrl Pts',(54.6631764277562,-44.3896643528756,47.6978257430375));
#15751=CARTESIAN_POINT('Ctrl Pts',(54.6969417294651,-44.3272645584125,47.6978257430375));
#15752=CARTESIAN_POINT('',(54.3870404098839,-44.8272645584125,51.5));
#15753=CARTESIAN_POINT('',(54.3870404098839,-44.8272645584125,64.));
#15754=CARTESIAN_POINT('',(53.9843998056396,-45.3272645584125,52.));
#15755=CARTESIAN_POINT('Ctrl Pts',(53.9843998056396,-45.3272645584125,52.));
#15756=CARTESIAN_POINT('Ctrl Pts',(54.0373751514369,-45.269501845417,52.));
#15757=CARTESIAN_POINT('Ctrl Pts',(54.09337665569,-45.2054409446566,51.9894566895945));
#15758=CARTESIAN_POINT('Ctrl Pts',(54.1960417034407,-45.0819180329636,51.9406971089121));
#15759=CARTESIAN_POINT('Ctrl Pts',(54.2427357823159,-45.0225259231798,51.9023681459539));
#15760=CARTESIAN_POINT('Ctrl Pts',(54.3112071685676,-44.9324583590974,51.8123005818715));
#15761=CARTESIAN_POINT('Ctrl Pts',(54.3393802752971,-44.8939359317371,51.7582688558033));
#15762=CARTESIAN_POINT('Ctrl Pts',(54.377261890984,-44.8412774147571,51.6352518100092));
#15763=CARTESIAN_POINT('Ctrl Pts',(54.3870404098839,-44.8272645584125,51.5662353407203));
#15764=CARTESIAN_POINT('Ctrl Pts',(54.3870404098839,-44.8272645584125,51.5));
#15765=CARTESIAN_POINT('',(46.6145232391052,-45.3272645584125,52.));
#15766=CARTESIAN_POINT('Origin',(50.2994615223724,-41.9477335482704,52.));
#15767=CARTESIAN_POINT('',(46.2118826348608,-44.8272645584125,51.5));
#15768=CARTESIAN_POINT('Ctrl Pts',(46.2118826348608,-44.8272645584125,51.5));
#15769=CARTESIAN_POINT('Ctrl Pts',(46.2118826348608,-44.8272645584125,51.5662353407203));
#15770=CARTESIAN_POINT('Ctrl Pts',(46.2216611537608,-44.8412774147571,51.6352518100092));
#15771=CARTESIAN_POINT('Ctrl Pts',(46.2595427694477,-44.8939359317371,51.7582688558033));
#15772=CARTESIAN_POINT('Ctrl Pts',(46.2877158761771,-44.9324583590974,51.8123005818715));
#15773=CARTESIAN_POINT('Ctrl Pts',(46.3561872624289,-45.0225259231798,51.9023681459539));
#15774=CARTESIAN_POINT('Ctrl Pts',(46.4028813413041,-45.0819180329636,51.9406971089121));
#15775=CARTESIAN_POINT('Ctrl Pts',(46.5055463890548,-45.2054409446566,51.9894566895945));
#15776=CARTESIAN_POINT('Ctrl Pts',(46.5615478933078,-45.269501845417,52.));
#15777=CARTESIAN_POINT('Ctrl Pts',(46.6145232391052,-45.3272645584125,52.));
#15778=CARTESIAN_POINT('',(46.2118826348608,-44.8272645584125,48.1978257430375));
#15779=CARTESIAN_POINT('',(46.2118826348608,-44.8272645584125,64.));
#15780=CARTESIAN_POINT('Ctrl Pts',(45.9019813152797,-44.3272645584125,47.6978257430375));
#15781=CARTESIAN_POINT('Ctrl Pts',(45.9357466169886,-44.3896643528756,47.6978257430375));
#15782=CARTESIAN_POINT('Ctrl Pts',(45.9734850996506,-44.4559300231492,47.710126421675));
#15783=CARTESIAN_POINT('Ctrl Pts',(46.0470422481974,-44.5787128115292,47.7605853033887));
#15784=CARTESIAN_POINT('Ctrl Pts',(46.0828134243267,-44.6352673224994,47.7987217259379));
#15785=CARTESIAN_POINT('Ctrl Pts',(46.140067742602,-44.7229773515989,47.8864317550374));
#15786=CARTESIAN_POINT('Ctrl Pts',(46.1661151586053,-44.7613527165994,47.9408836439009));
#15787=CARTESIAN_POINT('Ctrl Pts',(46.2021246042205,-44.8135380049881,48.0636994127672));
#15788=CARTESIAN_POINT('Ctrl Pts',(46.2118826348608,-44.8272645584125,48.1321584122493));
#15789=CARTESIAN_POINT('Ctrl Pts',(46.2118826348608,-44.8272645584125,48.1978257430375));
#15790=CARTESIAN_POINT('Origin',(-33.7005384776276,-0.052266451729599,64.));
#15791=CARTESIAN_POINT('',(-28.7005384776276,-0.0522664517295984,64.));
#15792=CARTESIAN_POINT('Origin',(-33.7005384776276,-0.052266451729599,64.));
#15793=CARTESIAN_POINT('',(-28.7005384776276,-0.0522664517295984,35.6978257430375));
#15794=CARTESIAN_POINT('',(-28.7005384776276,-0.0522664517295996,64.));
#15795=CARTESIAN_POINT('Origin',(-33.7005384776276,-0.052266451729599,35.6978257430375));
#15796=CARTESIAN_POINT('Origin',(50.2994615223724,-0.052266451729599,64.));
#15797=CARTESIAN_POINT('',(55.2994615223724,-0.0522664517295984,64.));
#15798=CARTESIAN_POINT('Origin',(50.2994615223724,-0.052266451729599,64.));
#15799=CARTESIAN_POINT('',(55.2994615223724,-0.0522664517295984,35.6978257430375));
#15800=CARTESIAN_POINT('',(55.2994615223724,-0.0522664517295996,64.));
#15801=CARTESIAN_POINT('Origin',(50.2994615223724,-0.052266451729599,35.6978257430375));
#15802=CARTESIAN_POINT('Origin',(71.2994615223724,-20.9477335482704,64.));
#15803=CARTESIAN_POINT('',(76.2994615223724,-20.9477335482704,64.));
#15804=CARTESIAN_POINT('Origin',(71.2994615223724,-20.9477335482704,64.));
#15805=CARTESIAN_POINT('',(76.2994615223724,-20.9477335482704,35.6978257430375));
#15806=CARTESIAN_POINT('',(76.2994615223724,-20.9477335482704,64.));
#15807=CARTESIAN_POINT('',(76.2978638949456,-21.0741207385024,35.6978257430375));
#15808=CARTESIAN_POINT('Origin',(71.2994615223724,-20.9477335482704,35.6978257430375));
#15809=CARTESIAN_POINT('',(76.2600702640404,-21.5741207385024,36.1978257430375));
#15810=CARTESIAN_POINT('Ctrl Pts',(76.2600702640404,-21.5741207385024,36.1978257430375));
#15811=CARTESIAN_POINT('Ctrl Pts',(76.2600702640404,-21.5741207385024,36.1349939529891));
#15812=CARTESIAN_POINT('Ctrl Pts',(76.261707444775,-21.5615536728765,36.0680174512863));
#15813=CARTESIAN_POINT('Ctrl Pts',(76.2677518597934,-21.5105397842088,35.9448840917433));
#15814=CARTESIAN_POINT('Ctrl Pts',(76.272089134882,-21.4720964497992,35.8887223643976));
#15815=CARTESIAN_POINT('Ctrl Pts',(76.2806427116048,-21.3834176983908,35.7999882651862));
#15816=CARTESIAN_POINT('Ctrl Pts',(76.285421251069,-21.3272274349036,35.7614956023605));
#15817=CARTESIAN_POINT('Ctrl Pts',(76.2932700900897,-21.2040263789334,35.7104126564947));
#15818=CARTESIAN_POINT('Ctrl Pts',(76.2962737086844,-21.1370099503463,35.6978257430375));
#15819=CARTESIAN_POINT('Ctrl Pts',(76.2978638949456,-21.0741207385024,35.6978257430375));
#15820=CARTESIAN_POINT('',(76.2600702640404,-21.5741207385024,47.1978257430375));
#15821=CARTESIAN_POINT('',(76.2600702640404,-21.5741207385024,64.));
#15822=CARTESIAN_POINT('Ctrl Pts',(76.1709348003122,-22.0741207385024,47.6978257430375));
#15823=CARTESIAN_POINT('Ctrl Pts',(76.1853501219146,-22.0117764091386,47.6978257430375));
#15824=CARTESIAN_POINT('Ctrl Pts',(76.1994330591515,-21.9448505322038,47.685440610641));
#15825=CARTESIAN_POINT('Ctrl Pts',(76.2229851313344,-21.8211627737637,47.6342788519733));
#15826=CARTESIAN_POINT('Ctrl Pts',(76.2325215699319,-21.7644213914886,47.5954836759127));
#15827=CARTESIAN_POINT('Ctrl Pts',(76.2463930261636,-21.6756387909071,47.5061996323312));
#15828=CARTESIAN_POINT('Ctrl Pts',(76.2517358957749,-21.6373959691348,47.4501913374276));
#15829=CARTESIAN_POINT('Ctrl Pts',(76.2585400256461,-21.5866358243642,47.3273455515029));
#15830=CARTESIAN_POINT('Ctrl Pts',(76.2600702640404,-21.5741207385024,47.2605109663339));
#15831=CARTESIAN_POINT('Ctrl Pts',(76.2600702640404,-21.5741207385024,47.1978257430375));
#15832=CARTESIAN_POINT('',(66.3388527807044,-21.5741207385024,47.1978257430375));
#15833=CARTESIAN_POINT('Ctrl Pts',(66.3388527807044,-21.5741207385024,47.1978257430375));
#15834=CARTESIAN_POINT('Ctrl Pts',(66.3388527807044,-21.5741207385024,47.2605109663339));
#15835=CARTESIAN_POINT('Ctrl Pts',(66.3403830190987,-21.5866358243642,47.3273455515029));
#15836=CARTESIAN_POINT('Ctrl Pts',(66.3471871489699,-21.6373959691348,47.4501913374276));
#15837=CARTESIAN_POINT('Ctrl Pts',(66.3525300185812,-21.6756387909071,47.5061996323312));
#15838=CARTESIAN_POINT('Ctrl Pts',(66.3664014748128,-21.7644213914886,47.5954836759127));
#15839=CARTESIAN_POINT('Ctrl Pts',(66.3759379134104,-21.8211627737637,47.6342788519733));
#15840=CARTESIAN_POINT('Ctrl Pts',(66.3994899855933,-21.9448505322038,47.6854406106411));
#15841=CARTESIAN_POINT('Ctrl Pts',(66.4135729228302,-22.0117764091386,47.6978257430375));
#15842=CARTESIAN_POINT('Ctrl Pts',(66.4279882444326,-22.0741207385024,47.6978257430375));
#15843=CARTESIAN_POINT('',(66.3388527807044,-21.5741207385024,36.1978257430375));
#15844=CARTESIAN_POINT('',(66.3388527807044,-21.5741207385024,64.));
#15845=CARTESIAN_POINT('',(66.3010591497992,-21.0741207385024,35.6978257430375));
#15846=CARTESIAN_POINT('Ctrl Pts',(66.3010591497992,-21.0741207385024,35.6978257430375));
#15847=CARTESIAN_POINT('Ctrl Pts',(66.3026493360604,-21.1370099503463,35.6978257430375));
#15848=CARTESIAN_POINT('Ctrl Pts',(66.305652954655,-21.2040263789334,35.7104126564947));
#15849=CARTESIAN_POINT('Ctrl Pts',(66.3135017936757,-21.3272274349036,35.7614956023605));
#15850=CARTESIAN_POINT('Ctrl Pts',(66.31828033314,-21.3834176983908,35.7999882651862));
#15851=CARTESIAN_POINT('Ctrl Pts',(66.3268339098628,-21.4720964497992,35.8887223643976));
#15852=CARTESIAN_POINT('Ctrl Pts',(66.3311711849514,-21.5105397842088,35.9448840917433));
#15853=CARTESIAN_POINT('Ctrl Pts',(66.3372155999698,-21.5615536728765,36.0680174512863));
#15854=CARTESIAN_POINT('Ctrl Pts',(66.3388527807044,-21.5741207385024,36.1349939529891));
#15855=CARTESIAN_POINT('Ctrl Pts',(66.3388527807044,-21.5741207385024,36.1978257430375));
#15856=CARTESIAN_POINT('Origin',(71.2994615223724,-20.9477335482704,35.6978257430375));
#15857=CARTESIAN_POINT('Origin',(71.2994615223724,45.9821613702938,64.));
#15858=CARTESIAN_POINT('',(83.7994615223724,45.9821613702938,64.));
#15859=CARTESIAN_POINT('Origin',(71.2994615223724,45.9821613702938,64.));
#15860=CARTESIAN_POINT('',(83.7994615223724,45.9821613702938,52.));
#15861=CARTESIAN_POINT('',(83.7994615223724,45.9821613702938,64.));
#15862=CARTESIAN_POINT('Origin',(71.2994615223724,45.9821613702938,52.));
#15863=CARTESIAN_POINT('Origin',(29.2994615223724,-20.9477335482704,64.));
#15864=CARTESIAN_POINT('',(34.2994615223724,-20.9477335482704,64.));
#15865=CARTESIAN_POINT('Origin',(29.2994615223724,-20.9477335482704,64.));
#15866=CARTESIAN_POINT('',(34.2994615223724,-20.9477335482704,35.6978257430375));
#15867=CARTESIAN_POINT('',(34.2994615223724,-20.9477335482704,64.));
#15868=CARTESIAN_POINT('',(34.2978638949456,-21.0741207385024,35.6978257430375));
#15869=CARTESIAN_POINT('Origin',(29.2994615223724,-20.9477335482704,35.6978257430375));
#15870=CARTESIAN_POINT('',(34.2600702640404,-21.5741207385024,36.1978257430375));
#15871=CARTESIAN_POINT('Ctrl Pts',(34.2600702640404,-21.5741207385024,36.1978257430375));
#15872=CARTESIAN_POINT('Ctrl Pts',(34.2600702640404,-21.5741207385024,36.1349939529891));
#15873=CARTESIAN_POINT('Ctrl Pts',(34.261707444775,-21.5615536728765,36.0680174512863));
#15874=CARTESIAN_POINT('Ctrl Pts',(34.2677518597934,-21.5105397842088,35.9448840917433));
#15875=CARTESIAN_POINT('Ctrl Pts',(34.272089134882,-21.4720964497992,35.8887223643976));
#15876=CARTESIAN_POINT('Ctrl Pts',(34.2806427116048,-21.3834176983908,35.7999882651862));
#15877=CARTESIAN_POINT('Ctrl Pts',(34.285421251069,-21.3272274349036,35.7614956023605));
#15878=CARTESIAN_POINT('Ctrl Pts',(34.2932700900897,-21.2040263789334,35.7104126564947));
#15879=CARTESIAN_POINT('Ctrl Pts',(34.2962737086844,-21.1370099503463,35.6978257430375));
#15880=CARTESIAN_POINT('Ctrl Pts',(34.2978638949456,-21.0741207385024,35.6978257430375));
#15881=CARTESIAN_POINT('',(34.2600702640404,-21.5741207385024,47.1978257430375));
#15882=CARTESIAN_POINT('',(34.2600702640404,-21.5741207385024,64.));
#15883=CARTESIAN_POINT('Ctrl Pts',(34.1709348003122,-22.0741207385024,47.6978257430375));
#15884=CARTESIAN_POINT('Ctrl Pts',(34.1853501219146,-22.0117764091386,47.6978257430375));
#15885=CARTESIAN_POINT('Ctrl Pts',(34.1994330591515,-21.9448505322038,47.6854406106411));
#15886=CARTESIAN_POINT('Ctrl Pts',(34.2229851313344,-21.8211627737637,47.6342788519733));
#15887=CARTESIAN_POINT('Ctrl Pts',(34.2325215699319,-21.7644213914886,47.5954836759127));
#15888=CARTESIAN_POINT('Ctrl Pts',(34.2463930261636,-21.6756387909071,47.5061996323312));
#15889=CARTESIAN_POINT('Ctrl Pts',(34.2517358957749,-21.6373959691348,47.4501913374276));
#15890=CARTESIAN_POINT('Ctrl Pts',(34.2585400256461,-21.5866358243642,47.3273455515029));
#15891=CARTESIAN_POINT('Ctrl Pts',(34.2600702640404,-21.5741207385024,47.2605109663339));
#15892=CARTESIAN_POINT('Ctrl Pts',(34.2600702640404,-21.5741207385024,47.1978257430375));
#15893=CARTESIAN_POINT('',(24.3388527807044,-21.5741207385024,47.1978257430375));
#15894=CARTESIAN_POINT('Ctrl Pts',(24.3388527807044,-21.5741207385024,47.1978257430375));
#15895=CARTESIAN_POINT('Ctrl Pts',(24.3388527807044,-21.5741207385024,47.2605109663339));
#15896=CARTESIAN_POINT('Ctrl Pts',(24.3403830190987,-21.5866358243642,47.3273455515029));
#15897=CARTESIAN_POINT('Ctrl Pts',(24.3471871489699,-21.6373959691348,47.4501913374276));
#15898=CARTESIAN_POINT('Ctrl Pts',(24.3525300185812,-21.6756387909071,47.5061996323312));
#15899=CARTESIAN_POINT('Ctrl Pts',(24.3664014748128,-21.7644213914886,47.5954836759127));
#15900=CARTESIAN_POINT('Ctrl Pts',(24.3759379134104,-21.8211627737637,47.6342788519733));
#15901=CARTESIAN_POINT('Ctrl Pts',(24.3994899855933,-21.9448505322038,47.6854406106411));
#15902=CARTESIAN_POINT('Ctrl Pts',(24.4135729228302,-22.0117764091386,47.6978257430375));
#15903=CARTESIAN_POINT('Ctrl Pts',(24.4279882444326,-22.0741207385024,47.6978257430375));
#15904=CARTESIAN_POINT('',(24.3388527807044,-21.5741207385024,36.1978257430375));
#15905=CARTESIAN_POINT('',(24.3388527807044,-21.5741207385024,64.));
#15906=CARTESIAN_POINT('',(24.3010591497992,-21.0741207385024,35.6978257430375));
#15907=CARTESIAN_POINT('Ctrl Pts',(24.3010591497992,-21.0741207385024,35.6978257430375));
#15908=CARTESIAN_POINT('Ctrl Pts',(24.3026493360604,-21.1370099503463,35.6978257430375));
#15909=CARTESIAN_POINT('Ctrl Pts',(24.305652954655,-21.2040263789334,35.7104126564947));
#15910=CARTESIAN_POINT('Ctrl Pts',(24.3135017936757,-21.3272274349036,35.7614956023605));
#15911=CARTESIAN_POINT('Ctrl Pts',(24.31828033314,-21.3834176983908,35.7999882651862));
#15912=CARTESIAN_POINT('Ctrl Pts',(24.3268339098628,-21.4720964497992,35.8887223643976));
#15913=CARTESIAN_POINT('Ctrl Pts',(24.3311711849514,-21.5105397842088,35.9448840917433));
#15914=CARTESIAN_POINT('Ctrl Pts',(24.3372155999698,-21.5615536728765,36.0680174512863));
#15915=CARTESIAN_POINT('Ctrl Pts',(24.3388527807044,-21.5741207385024,36.1349939529891));
#15916=CARTESIAN_POINT('Ctrl Pts',(24.3388527807044,-21.5741207385024,36.1978257430375));
#15917=CARTESIAN_POINT('Origin',(29.2994615223724,-20.9477335482704,35.6978257430375));
#15918=CARTESIAN_POINT('Origin',(8.29946152237238,-0.052266451729599,64.));
#15919=CARTESIAN_POINT('',(13.2994615223724,-0.0522664517295984,64.));
#15920=CARTESIAN_POINT('Origin',(8.29946152237238,-0.052266451729599,64.));
#15921=CARTESIAN_POINT('',(13.2994615223724,-0.0522664517295984,35.6978257430375));
#15922=CARTESIAN_POINT('',(13.2994615223724,-0.0522664517295996,64.));
#15923=CARTESIAN_POINT('Origin',(8.29946152237238,-0.052266451729599,35.6978257430375));
#15924=CARTESIAN_POINT('Origin',(-54.7005384776276,-20.9477335482704,64.));
#15925=CARTESIAN_POINT('',(-49.7005384776276,-20.9477335482704,64.));
#15926=CARTESIAN_POINT('Origin',(-54.7005384776276,-20.9477335482704,64.));
#15927=CARTESIAN_POINT('',(-49.7005384776276,-20.9477335482704,35.6978257430375));
#15928=CARTESIAN_POINT('',(-49.7005384776276,-20.9477335482704,64.));
#15929=CARTESIAN_POINT('',(-49.7021361050544,-21.0741207385024,35.6978257430375));
#15930=CARTESIAN_POINT('Origin',(-54.7005384776276,-20.9477335482704,35.6978257430375));
#15931=CARTESIAN_POINT('',(-49.7399297359596,-21.5741207385024,36.1978257430375));
#15932=CARTESIAN_POINT('Ctrl Pts',(-49.7399297359596,-21.5741207385024,
36.1978257430375));
#15933=CARTESIAN_POINT('Ctrl Pts',(-49.7399297359596,-21.5741207385024,
36.1349939529891));
#15934=CARTESIAN_POINT('Ctrl Pts',(-49.738292555225,-21.5615536728765,36.0680174512863));
#15935=CARTESIAN_POINT('Ctrl Pts',(-49.7322481402066,-21.5105397842088,
35.9448840917433));
#15936=CARTESIAN_POINT('Ctrl Pts',(-49.727910865118,-21.4720964497991,35.8887223643976));
#15937=CARTESIAN_POINT('Ctrl Pts',(-49.7193572883952,-21.3834176983908,
35.7999882651862));
#15938=CARTESIAN_POINT('Ctrl Pts',(-49.714578748931,-21.3272274349035,35.7614956023605));
#15939=CARTESIAN_POINT('Ctrl Pts',(-49.7067299099103,-21.2040263789334,
35.7104126564947));
#15940=CARTESIAN_POINT('Ctrl Pts',(-49.7037262913156,-21.1370099503463,
35.6978257430375));
#15941=CARTESIAN_POINT('Ctrl Pts',(-49.7021361050544,-21.0741207385024,
35.6978257430375));
#15942=CARTESIAN_POINT('',(-49.7399297359596,-21.5741207385024,47.1978257430375));
#15943=CARTESIAN_POINT('',(-49.7399297359596,-21.5741207385024,64.));
#15944=CARTESIAN_POINT('Ctrl Pts',(-49.8290651996878,-22.0741207385024,
47.6978257430375));
#15945=CARTESIAN_POINT('Ctrl Pts',(-49.8146498780854,-22.0117764091386,
47.6978257430375));
#15946=CARTESIAN_POINT('Ctrl Pts',(-49.8005669408485,-21.9448505322038,
47.6854406106411));
#15947=CARTESIAN_POINT('Ctrl Pts',(-49.7770148686656,-21.8211627737637,
47.6342788519733));
#15948=CARTESIAN_POINT('Ctrl Pts',(-49.7674784300681,-21.7644213914886,
47.5954836759127));
#15949=CARTESIAN_POINT('Ctrl Pts',(-49.7536069738364,-21.675638790907,47.5061996323312));
#15950=CARTESIAN_POINT('Ctrl Pts',(-49.7482641042251,-21.6373959691347,
47.4501913374276));
#15951=CARTESIAN_POINT('Ctrl Pts',(-49.7414599743539,-21.5866358243642,
47.3273455515029));
#15952=CARTESIAN_POINT('Ctrl Pts',(-49.7399297359596,-21.5741207385024,
47.2605109663339));
#15953=CARTESIAN_POINT('Ctrl Pts',(-49.7399297359596,-21.5741207385024,
47.1978257430375));
#15954=CARTESIAN_POINT('',(-59.6611472192956,-21.5741207385024,47.1978257430375));
#15955=CARTESIAN_POINT('Ctrl Pts',(-59.6611472192956,-21.5741207385024,
47.1978257430375));
#15956=CARTESIAN_POINT('Ctrl Pts',(-59.6611472192956,-21.5741207385024,
47.2605109663339));
#15957=CARTESIAN_POINT('Ctrl Pts',(-59.6596169809013,-21.5866358243642,
47.3273455515029));
#15958=CARTESIAN_POINT('Ctrl Pts',(-59.6528128510301,-21.6373959691347,
47.4501913374276));
#15959=CARTESIAN_POINT('Ctrl Pts',(-59.6474699814188,-21.675638790907,47.5061996323312));
#15960=CARTESIAN_POINT('Ctrl Pts',(-59.6335985251872,-21.7644213914886,
47.5954836759127));
#15961=CARTESIAN_POINT('Ctrl Pts',(-59.6240620865897,-21.8211627737637,
47.6342788519733));
#15962=CARTESIAN_POINT('Ctrl Pts',(-59.6005100144067,-21.9448505322038,
47.6854406106411));
#15963=CARTESIAN_POINT('Ctrl Pts',(-59.5864270771698,-22.0117764091386,
47.6978257430375));
#15964=CARTESIAN_POINT('Ctrl Pts',(-59.5720117555674,-22.0741207385024,
47.6978257430375));
#15965=CARTESIAN_POINT('',(-59.6611472192956,-21.5741207385024,36.1978257430375));
#15966=CARTESIAN_POINT('',(-59.6611472192956,-21.5741207385024,64.));
#15967=CARTESIAN_POINT('',(-59.6989408502008,-21.0741207385024,35.6978257430375));
#15968=CARTESIAN_POINT('Ctrl Pts',(-59.6989408502008,-21.0741207385024,
35.6978257430375));
#15969=CARTESIAN_POINT('Ctrl Pts',(-59.6973506639396,-21.1370099503463,
35.6978257430375));
#15970=CARTESIAN_POINT('Ctrl Pts',(-59.694347045345,-21.2040263789334,35.7104126564947));
#15971=CARTESIAN_POINT('Ctrl Pts',(-59.6864982063243,-21.3272274349035,
35.7614956023605));
#15972=CARTESIAN_POINT('Ctrl Pts',(-59.68171966686,-21.3834176983908,35.7999882651862));
#15973=CARTESIAN_POINT('Ctrl Pts',(-59.6731660901373,-21.4720964497991,
35.8887223643976));
#15974=CARTESIAN_POINT('Ctrl Pts',(-59.6688288150486,-21.5105397842088,
35.9448840917433));
#15975=CARTESIAN_POINT('Ctrl Pts',(-59.6627844000302,-21.5615536728765,
36.0680174512863));
#15976=CARTESIAN_POINT('Ctrl Pts',(-59.6611472192956,-21.5741207385024,
36.1349939529891));
#15977=CARTESIAN_POINT('Ctrl Pts',(-59.6611472192956,-21.5741207385024,
36.1978257430375));
#15978=CARTESIAN_POINT('Origin',(-54.7005384776276,-20.9477335482704,35.6978257430375));
#15979=CARTESIAN_POINT('Origin',(-33.7005384776276,41.9477335482704,64.));
#15980=CARTESIAN_POINT('',(-28.7005384776276,41.9477335482704,64.));
#15981=CARTESIAN_POINT('Origin',(-33.7005384776276,41.9477335482704,64.));
#15982=CARTESIAN_POINT('',(-28.7005384776276,41.9477335482704,52.));
#15983=CARTESIAN_POINT('',(-28.7005384776276,41.9477335482704,64.));
#15984=CARTESIAN_POINT('Origin',(-33.7005384776276,41.9477335482704,52.));
#15985=CARTESIAN_POINT('Origin',(8.29946152237238,-41.9477335482704,64.));
#15986=CARTESIAN_POINT('',(13.2994615223724,-41.9477335482704,64.));
#15987=CARTESIAN_POINT('Origin',(8.29946152237238,-41.9477335482704,64.));
#15988=CARTESIAN_POINT('',(13.2994615223724,-41.9477335482704,64.));
#15989=CARTESIAN_POINT('',(12.387040409884,-44.8272645584125,48.1978257430375));
#15990=CARTESIAN_POINT('Ctrl Pts',(12.3870404098839,-44.8272645584125,48.1978257430375));
#15991=CARTESIAN_POINT('Ctrl Pts',(12.3870404098839,-44.8272645584125,48.1321584122493));
#15992=CARTESIAN_POINT('Ctrl Pts',(12.3967984405243,-44.8135380049881,48.0636994127671));
#15993=CARTESIAN_POINT('Ctrl Pts',(12.4328078861395,-44.7613527165994,47.9408836439009));
#15994=CARTESIAN_POINT('Ctrl Pts',(12.4588553021428,-44.7229773515989,47.8864317550374));
#15995=CARTESIAN_POINT('Ctrl Pts',(12.516109620418,-44.6352673224994,47.7987217259379));
#15996=CARTESIAN_POINT('Ctrl Pts',(12.5518807965474,-44.5787128115292,47.7605853033887));
#15997=CARTESIAN_POINT('Ctrl Pts',(12.6254379450942,-44.4559300231491,47.710126421675));
#15998=CARTESIAN_POINT('Ctrl Pts',(12.6631764277562,-44.3896643528756,47.6978257430375));
#15999=CARTESIAN_POINT('Ctrl Pts',(12.6969417294651,-44.3272645584124,47.6978257430375));
#16000=CARTESIAN_POINT('',(12.3870404098839,-44.8272645584125,51.5));
#16001=CARTESIAN_POINT('',(12.387040409884,-44.8272645584125,64.));
#16002=CARTESIAN_POINT('',(11.9843998056396,-45.3272645584125,52.));
#16003=CARTESIAN_POINT('Ctrl Pts',(11.9843998056396,-45.3272645584125,52.));
#16004=CARTESIAN_POINT('Ctrl Pts',(12.0373751514369,-45.269501845417,52.));
#16005=CARTESIAN_POINT('Ctrl Pts',(12.09337665569,-45.2054409446566,51.9894566895945));
#16006=CARTESIAN_POINT('Ctrl Pts',(12.1960417034407,-45.0819180329636,51.9406971089121));
#16007=CARTESIAN_POINT('Ctrl Pts',(12.2427357823159,-45.0225259231798,51.9023681459539));
#16008=CARTESIAN_POINT('Ctrl Pts',(12.3112071685676,-44.9324583590974,51.8123005818715));
#16009=CARTESIAN_POINT('Ctrl Pts',(12.3393802752971,-44.8939359317371,51.7582688558033));
#16010=CARTESIAN_POINT('Ctrl Pts',(12.377261890984,-44.8412774147571,51.6352518100092));
#16011=CARTESIAN_POINT('Ctrl Pts',(12.387040409884,-44.8272645584125,51.5662353407203));
#16012=CARTESIAN_POINT('Ctrl Pts',(12.387040409884,-44.8272645584125,51.5));
#16013=CARTESIAN_POINT('',(4.61452323910518,-45.3272645584125,52.));
#16014=CARTESIAN_POINT('Origin',(8.29946152237238,-41.9477335482704,52.));
#16015=CARTESIAN_POINT('',(4.21188263486082,-44.8272645584125,51.5));
#16016=CARTESIAN_POINT('Ctrl Pts',(4.21188263486082,-44.8272645584125,51.5));
#16017=CARTESIAN_POINT('Ctrl Pts',(4.21188263486082,-44.8272645584125,51.5662353407203));
#16018=CARTESIAN_POINT('Ctrl Pts',(4.22166115376081,-44.8412774147571,51.6352518100092));
#16019=CARTESIAN_POINT('Ctrl Pts',(4.25954276944767,-44.8939359317371,51.7582688558033));
#16020=CARTESIAN_POINT('Ctrl Pts',(4.28771587617714,-44.9324583590974,51.8123005818715));
#16021=CARTESIAN_POINT('Ctrl Pts',(4.3561872624289,-45.0225259231798,51.9023681459539));
#16022=CARTESIAN_POINT('Ctrl Pts',(4.40288134130409,-45.0819180329636,51.9406971089121));
#16023=CARTESIAN_POINT('Ctrl Pts',(4.50554638905476,-45.2054409446566,51.9894566895945));
#16024=CARTESIAN_POINT('Ctrl Pts',(4.56154789330784,-45.269501845417,52.));
#16025=CARTESIAN_POINT('Ctrl Pts',(4.61452323910518,-45.3272645584125,52.));
#16026=CARTESIAN_POINT('',(4.21188263486082,-44.8272645584125,48.1978257430375));
#16027=CARTESIAN_POINT('',(4.21188263486082,-44.8272645584125,64.));
#16028=CARTESIAN_POINT('Ctrl Pts',(3.90198131527965,-44.3272645584124,47.6978257430375));
#16029=CARTESIAN_POINT('Ctrl Pts',(3.93574661698859,-44.3896643528756,47.6978257430375));
#16030=CARTESIAN_POINT('Ctrl Pts',(3.97348509965058,-44.4559300231491,47.710126421675));
#16031=CARTESIAN_POINT('Ctrl Pts',(4.04704224819734,-44.5787128115292,47.7605853033887));
#16032=CARTESIAN_POINT('Ctrl Pts',(4.08281342432674,-44.6352673224994,47.7987217259379));
#16033=CARTESIAN_POINT('Ctrl Pts',(4.14006774260197,-44.7229773515989,47.8864317550374));
#16034=CARTESIAN_POINT('Ctrl Pts',(4.16611515860529,-44.7613527165994,47.9408836439009));
#16035=CARTESIAN_POINT('Ctrl Pts',(4.20212460422049,-44.8135380049881,48.0636994127672));
#16036=CARTESIAN_POINT('Ctrl Pts',(4.21188263486082,-44.8272645584125,48.1321584122493));
#16037=CARTESIAN_POINT('Ctrl Pts',(4.21188263486082,-44.8272645584125,48.1978257430375));
#16038=CARTESIAN_POINT('Origin',(50.2994615223724,41.9477335482704,64.));
#16039=CARTESIAN_POINT('',(55.2994615223724,41.9477335482704,64.));
#16040=CARTESIAN_POINT('Origin',(50.2994615223724,41.9477335482704,64.));
#16041=CARTESIAN_POINT('',(55.2994615223724,41.9477335482704,52.));
#16042=CARTESIAN_POINT('',(55.2994615223724,41.9477335482704,64.));
#16043=CARTESIAN_POINT('Origin',(50.2994615223724,41.9477335482704,52.));
#16044=CARTESIAN_POINT('Origin',(-12.7005384776276,-20.9477335482704,64.));
#16045=CARTESIAN_POINT('',(-7.70053847762761,-20.9477335482704,64.));
#16046=CARTESIAN_POINT('Origin',(-12.7005384776276,-20.9477335482704,64.));
#16047=CARTESIAN_POINT('',(-7.70053847762761,-20.9477335482704,35.6978257430375));
#16048=CARTESIAN_POINT('',(-7.70053847762761,-20.9477335482704,64.));
#16049=CARTESIAN_POINT('',(-7.70213610505443,-21.0741207385024,35.6978257430375));
#16050=CARTESIAN_POINT('Origin',(-12.7005384776276,-20.9477335482704,35.6978257430375));
#16051=CARTESIAN_POINT('',(-7.73992973595958,-21.5741207385024,36.1978257430375));
#16052=CARTESIAN_POINT('Ctrl Pts',(-7.73992973595958,-21.5741207385024,
36.1978257430375));
#16053=CARTESIAN_POINT('Ctrl Pts',(-7.73992973595958,-21.5741207385024,
36.1349939529891));
#16054=CARTESIAN_POINT('Ctrl Pts',(-7.73829255522502,-21.5615536728765,
36.0680174512863));
#16055=CARTESIAN_POINT('Ctrl Pts',(-7.73224814020658,-21.5105397842088,
35.9448840917433));
#16056=CARTESIAN_POINT('Ctrl Pts',(-7.72791086511798,-21.4720964497992,
35.8887223643976));
#16057=CARTESIAN_POINT('Ctrl Pts',(-7.71935728839523,-21.3834176983908,
35.7999882651862));
#16058=CARTESIAN_POINT('Ctrl Pts',(-7.71457874893097,-21.3272274349035,
35.7614956023605));
#16059=CARTESIAN_POINT('Ctrl Pts',(-7.70672990991027,-21.2040263789334,
35.7104126564947));
#16060=CARTESIAN_POINT('Ctrl Pts',(-7.70372629131563,-21.1370099503463,
35.6978257430375));
#16061=CARTESIAN_POINT('Ctrl Pts',(-7.70213610505443,-21.0741207385024,
35.6978257430375));
#16062=CARTESIAN_POINT('',(-7.73992973595958,-21.5741207385024,47.1978257430375));
#16063=CARTESIAN_POINT('',(-7.73992973595958,-21.5741207385024,64.));
#16064=CARTESIAN_POINT('Ctrl Pts',(-7.82906519968783,-22.0741207385024,
47.6978257430375));
#16065=CARTESIAN_POINT('Ctrl Pts',(-7.81464987808543,-22.0117764091386,
47.6978257430375));
#16066=CARTESIAN_POINT('Ctrl Pts',(-7.80056694084853,-21.9448505322038,
47.6854406106411));
#16067=CARTESIAN_POINT('Ctrl Pts',(-7.77701486866557,-21.8211627737637,
47.6342788519733));
#16068=CARTESIAN_POINT('Ctrl Pts',(-7.76747843006806,-21.7644213914886,
47.5954836759127));
#16069=CARTESIAN_POINT('Ctrl Pts',(-7.7536069738364,-21.675638790907,47.5061996323312));
#16070=CARTESIAN_POINT('Ctrl Pts',(-7.74826410422513,-21.6373959691348,
47.4501913374276));
#16071=CARTESIAN_POINT('Ctrl Pts',(-7.74145997435394,-21.5866358243642,
47.3273455515029));
#16072=CARTESIAN_POINT('Ctrl Pts',(-7.73992973595958,-21.5741207385024,
47.2605109663339));
#16073=CARTESIAN_POINT('Ctrl Pts',(-7.73992973595958,-21.5741207385024,
47.1978257430375));
#16074=CARTESIAN_POINT('',(-17.6611472192956,-21.5741207385024,47.1978257430375));
#16075=CARTESIAN_POINT('Ctrl Pts',(-17.6611472192956,-21.5741207385024,
47.1978257430375));
#16076=CARTESIAN_POINT('Ctrl Pts',(-17.6611472192956,-21.5741207385024,
47.2605109663339));
#16077=CARTESIAN_POINT('Ctrl Pts',(-17.6596169809013,-21.5866358243642,
47.3273455515029));
#16078=CARTESIAN_POINT('Ctrl Pts',(-17.6528128510301,-21.6373959691348,
47.4501913374276));
#16079=CARTESIAN_POINT('Ctrl Pts',(-17.6474699814188,-21.675638790907,47.5061996323312));
#16080=CARTESIAN_POINT('Ctrl Pts',(-17.6335985251872,-21.7644213914886,
47.5954836759127));
#16081=CARTESIAN_POINT('Ctrl Pts',(-17.6240620865897,-21.8211627737637,
47.6342788519733));
#16082=CARTESIAN_POINT('Ctrl Pts',(-17.6005100144067,-21.9448505322038,
47.6854406106411));
#16083=CARTESIAN_POINT('Ctrl Pts',(-17.5864270771698,-22.0117764091386,
47.6978257430375));
#16084=CARTESIAN_POINT('Ctrl Pts',(-17.5720117555674,-22.0741207385024,
47.6978257430375));
#16085=CARTESIAN_POINT('',(-17.6611472192956,-21.5741207385024,36.1978257430375));
#16086=CARTESIAN_POINT('',(-17.6611472192956,-21.5741207385024,64.));
#16087=CARTESIAN_POINT('',(-17.6989408502008,-21.0741207385024,35.6978257430375));
#16088=CARTESIAN_POINT('Ctrl Pts',(-17.6989408502008,-21.0741207385024,
35.6978257430375));
#16089=CARTESIAN_POINT('Ctrl Pts',(-17.6973506639396,-21.1370099503463,
35.6978257430375));
#16090=CARTESIAN_POINT('Ctrl Pts',(-17.694347045345,-21.2040263789334,35.7104126564947));
#16091=CARTESIAN_POINT('Ctrl Pts',(-17.6864982063243,-21.3272274349035,
35.7614956023605));
#16092=CARTESIAN_POINT('Ctrl Pts',(-17.68171966686,-21.3834176983908,35.7999882651862));
#16093=CARTESIAN_POINT('Ctrl Pts',(-17.6731660901372,-21.4720964497992,
35.8887223643976));
#16094=CARTESIAN_POINT('Ctrl Pts',(-17.6688288150486,-21.5105397842088,
35.9448840917433));
#16095=CARTESIAN_POINT('Ctrl Pts',(-17.6627844000302,-21.5615536728765,
36.0680174512863));
#16096=CARTESIAN_POINT('Ctrl Pts',(-17.6611472192956,-21.5741207385024,
36.1349939529891));
#16097=CARTESIAN_POINT('Ctrl Pts',(-17.6611472192956,-21.5741207385024,
36.1978257430375));
#16098=CARTESIAN_POINT('Origin',(-12.7005384776276,-20.9477335482704,35.6978257430375));
#16099=CARTESIAN_POINT('Origin',(29.2994615223724,20.9477335482704,64.));
#16100=CARTESIAN_POINT('',(34.2994615223724,20.9477335482704,64.));
#16101=CARTESIAN_POINT('Origin',(29.2994615223724,20.9477335482704,64.));
#16102=CARTESIAN_POINT('',(34.2994615223724,20.9477335482704,47.6978257430375));
#16103=CARTESIAN_POINT('',(34.2994615223724,20.9477335482704,64.));
#16104=CARTESIAN_POINT('',(34.0987510891795,19.545300072509,47.6978257430375));
#16105=CARTESIAN_POINT('Origin',(29.2994615223724,20.9477335482704,47.6978257430375));
#16106=CARTESIAN_POINT('',(33.9233934931417,19.045300072509,47.1978257430375));
#16107=CARTESIAN_POINT('Ctrl Pts',(33.9233934931417,19.045300072509,47.1978257430375));
#16108=CARTESIAN_POINT('Ctrl Pts',(33.9233934931417,19.045300072509,47.2606262015597));
#16109=CARTESIAN_POINT('Ctrl Pts',(33.9286235220756,19.0578693331568,47.3272049658121));
#16110=CARTESIAN_POINT('Ctrl Pts',(33.9487439245958,19.1079235845375,47.4488825757172));
#16111=CARTESIAN_POINT('Ctrl Pts',(33.9635333627505,19.1453760973014,47.50401144732));
#16112=CARTESIAN_POINT('Ctrl Pts',(33.9963894622215,19.2327496876229,47.5933468507728));
#16113=CARTESIAN_POINT('Ctrl Pts',(34.0169336674918,19.2894923661088,47.6326971370671));
#16114=CARTESIAN_POINT('Ctrl Pts',(34.0588328495999,19.4138848506455,47.6849404681153));
#16115=CARTESIAN_POINT('Ctrl Pts',(34.0801249019844,19.4815591055255,47.6978257430375));
#16116=CARTESIAN_POINT('Ctrl Pts',(34.0987510891795,19.545300072509,47.6978257430375));
#16117=CARTESIAN_POINT('',(33.9233934931417,19.045300072509,36.1978257430375));
#16118=CARTESIAN_POINT('',(33.9233934931417,19.045300072509,64.));
#16119=CARTESIAN_POINT('',(33.6844716015559,18.545300072509,35.6978257430375));
#16120=CARTESIAN_POINT('Ctrl Pts',(33.6844716015559,18.545300072509,35.6978257430375));
#16121=CARTESIAN_POINT('Ctrl Pts',(33.7183437123576,18.6071246969023,35.6978257430375));
#16122=CARTESIAN_POINT('Ctrl Pts',(33.7533284422121,18.6744087742692,35.7099831569546));
#16123=CARTESIAN_POINT('Ctrl Pts',(33.8154443123393,18.800447936422,35.7624419799854));
#16124=CARTESIAN_POINT('Ctrl Pts',(33.8426335478405,18.8591453590194,35.8028130850757));
#16125=CARTESIAN_POINT('Ctrl Pts',(33.8819451449858,18.9470131641942,35.8942412268742));
#16126=CARTESIAN_POINT('Ctrl Pts',(33.8976695801488,18.983759545124,35.9488335262825));
#16127=CARTESIAN_POINT('Ctrl Pts',(33.91835801237,19.0329211748031,36.0694921472959));
#16128=CARTESIAN_POINT('Ctrl Pts',(33.9233934931417,19.045300072509,36.1355610097978));
#16129=CARTESIAN_POINT('Ctrl Pts',(33.9233934931417,19.045300072509,36.1978257430375));
#16130=CARTESIAN_POINT('',(24.9144514431889,18.545300072509,35.6978257430375));
#16131=CARTESIAN_POINT('Origin',(29.2994615223724,20.9477335482704,35.6978257430375));
#16132=CARTESIAN_POINT('',(24.6755295516031,19.045300072509,36.1978257430375));
#16133=CARTESIAN_POINT('Ctrl Pts',(24.6755295516031,19.045300072509,36.1978257430375));
#16134=CARTESIAN_POINT('Ctrl Pts',(24.6755295516031,19.045300072509,36.1355610097978));
#16135=CARTESIAN_POINT('Ctrl Pts',(24.6805650323748,19.0329211748031,36.0694921472959));
#16136=CARTESIAN_POINT('Ctrl Pts',(24.701253464596,18.983759545124,35.9488335262825));
#16137=CARTESIAN_POINT('Ctrl Pts',(24.716977899759,18.9470131641942,35.8942412268742));
#16138=CARTESIAN_POINT('Ctrl Pts',(24.7562894969043,18.8591453590194,35.8028130850757));
#16139=CARTESIAN_POINT('Ctrl Pts',(24.7834787324055,18.800447936422,35.7624419799854));
#16140=CARTESIAN_POINT('Ctrl Pts',(24.8455946025327,18.6744087742692,35.7099831569546));
#16141=CARTESIAN_POINT('Ctrl Pts',(24.8805793323871,18.6071246969023,35.6978257430375));
#16142=CARTESIAN_POINT('Ctrl Pts',(24.9144514431889,18.545300072509,35.6978257430375));
#16143=CARTESIAN_POINT('',(24.6755295516031,19.045300072509,47.1978257430375));
#16144=CARTESIAN_POINT('',(24.6755295516031,19.045300072509,64.));
#16145=CARTESIAN_POINT('',(24.5001719555652,19.545300072509,47.6978257430375));
#16146=CARTESIAN_POINT('Ctrl Pts',(24.5001719555652,19.545300072509,47.6978257430375));
#16147=CARTESIAN_POINT('Ctrl Pts',(24.5187981427604,19.4815591055255,47.6978257430375));
#16148=CARTESIAN_POINT('Ctrl Pts',(24.5400901951449,19.4138848506455,47.6849404681153));
#16149=CARTESIAN_POINT('Ctrl Pts',(24.5819893772529,19.2894923661088,47.6326971370671));
#16150=CARTESIAN_POINT('Ctrl Pts',(24.6025335825232,19.2327496876229,47.5933468507728));
#16151=CARTESIAN_POINT('Ctrl Pts',(24.6353896819943,19.1453760973014,47.50401144732));
#16152=CARTESIAN_POINT('Ctrl Pts',(24.6501791201489,19.1079235845375,47.4488825757172));
#16153=CARTESIAN_POINT('Ctrl Pts',(24.6702995226691,19.0578693331568,47.3272049658121));
#16154=CARTESIAN_POINT('Ctrl Pts',(24.6755295516031,19.045300072509,47.2606262015597));
#16155=CARTESIAN_POINT('Ctrl Pts',(24.6755295516031,19.045300072509,47.1978257430375));
#16156=CARTESIAN_POINT('',(26.2727417324721,24.92755355845,47.6978257430375));
#16157=CARTESIAN_POINT('Origin',(29.2994615223724,20.9477335482704,47.6978257430375));
#16158=CARTESIAN_POINT('',(26.8050928708948,25.2811069490433,48.5513791336308));
#16159=CARTESIAN_POINT('Ctrl Pts',(26.8050928708948,25.2811069490433,48.5513791336308));
#16160=CARTESIAN_POINT('Ctrl Pts',(26.82943543518,25.2951189723872,48.5373671102869));
#16161=CARTESIAN_POINT('Ctrl Pts',(26.8530498914274,25.308437537607,48.5223873647648));
#16162=CARTESIAN_POINT('Ctrl Pts',(26.9248328641831,25.348221870878,48.4716633740189));
#16163=CARTESIAN_POINT('Ctrl Pts',(26.9755840167052,25.3750874905218,48.4276121965828));
#16164=CARTESIAN_POINT('Ctrl Pts',(27.0333153241737,25.4047562084472,48.3496563433172));
#16165=CARTESIAN_POINT('Ctrl Pts',(27.0494846243196,25.4129061770103,48.3217082903646));
#16166=CARTESIAN_POINT('Ctrl Pts',(27.0722400173048,25.4242998143135,48.2623093314405));
#16167=CARTESIAN_POINT('Ctrl Pts',(27.078828127056,25.42755355845,48.2308611312278));
#16168=CARTESIAN_POINT('Ctrl Pts',(27.078828127056,25.42755355845,48.1978257430375));
#16169=CARTESIAN_POINT('Ctrl Pts',(27.078828127056,25.42755355845,48.1647903548472));
#16170=CARTESIAN_POINT('Ctrl Pts',(27.0722400173048,25.4242998143135,48.1333421546345));
#16171=CARTESIAN_POINT('Ctrl Pts',(27.0494846243196,25.4129061770103,48.0739431957104));
#16172=CARTESIAN_POINT('Ctrl Pts',(27.0333153241737,25.4047562084472,48.0459951427578));
#16173=CARTESIAN_POINT('Ctrl Pts',(26.9755840167052,25.3750874905218,47.9680392894922));
#16174=CARTESIAN_POINT('Ctrl Pts',(26.9248328641832,25.348221870878,47.9239881120561));
#16175=CARTESIAN_POINT('Ctrl Pts',(26.7868075959158,25.2717240182291,47.8264553384537));
#16176=CARTESIAN_POINT('Ctrl Pts',(26.6830441955061,25.2103549049237,47.7786797574698));
#16177=CARTESIAN_POINT('Ctrl Pts',(26.4736085973111,25.0744920557659,47.7140189797529));
#16178=CARTESIAN_POINT('Ctrl Pts',(26.3678144401405,24.9998579453427,47.6978257430375));
#16179=CARTESIAN_POINT('Ctrl Pts',(26.2727417324721,24.92755355845,47.6978257430375));
#16180=CARTESIAN_POINT('',(24.6113603597352,22.6860394732673,51.1464466094067));
#16181=CARTESIAN_POINT('Origin',(29.2994615223724,20.9477335482704,52.8847525344037));
#16182=CARTESIAN_POINT('',(24.7580823702008,23.0395928638606,52.));
#16183=CARTESIAN_POINT('Ctrl Pts',(24.7580823702008,23.0395928638606,52.));
#16184=CARTESIAN_POINT('Ctrl Pts',(24.7295403892111,22.9776288701721,52.));
#16185=CARTESIAN_POINT('Ctrl Pts',(24.7003039670753,22.9104700099307,51.9877768144645));
#16186=CARTESIAN_POINT('Ctrl Pts',(24.6488415484994,22.7852096676192,51.9357615493743));
#16187=CARTESIAN_POINT('Ctrl Pts',(24.6265540100987,22.7271564800506,51.8959141016255));
#16188=CARTESIAN_POINT('Ctrl Pts',(24.5939647498949,22.6389806710746,51.8052231982866));
#16189=CARTESIAN_POINT('Ctrl Pts',(24.5808795048891,22.6017210834816,51.7501423324695));
#16190=CARTESIAN_POINT('Ctrl Pts',(24.5637493585117,22.5520157275868,51.6287300770116));
#16191=CARTESIAN_POINT('Ctrl Pts',(24.5596319980784,22.5395928638606,51.5623995455887));
#16192=CARTESIAN_POINT('Ctrl Pts',(24.5596319980784,22.5395928638606,51.4376004544113));
#16193=CARTESIAN_POINT('Ctrl Pts',(24.5637493585117,22.5520157275868,51.3712699229884));
#16194=CARTESIAN_POINT('Ctrl Pts',(24.5808795048891,22.6017210834816,51.2498576675305));
#16195=CARTESIAN_POINT('Ctrl Pts',(24.5939647498949,22.6389806710746,51.1947768017134));
#16196=CARTESIAN_POINT('Ctrl Pts',(24.6101358897808,22.6827344516939,51.1497750043391));
#16197=CARTESIAN_POINT('Ctrl Pts',(24.610744984223,22.6843798444226,51.1481062382515));
#16198=CARTESIAN_POINT('Ctrl Pts',(24.6113603597352,22.6860394732673,51.1464466094067));
#16199=CARTESIAN_POINT('',(33.8408406745439,23.0395928638606,52.));
#16200=CARTESIAN_POINT('Origin',(29.2994615223724,20.9477335482704,52.));
#16201=CARTESIAN_POINT('',(33.9875626850096,22.6860394732673,51.1464466094067));
#16202=CARTESIAN_POINT('Ctrl Pts',(33.9875626850096,22.6860394732673,51.1464466094067));
#16203=CARTESIAN_POINT('Ctrl Pts',(33.9881780605218,22.6843798444226,51.1481062382515));
#16204=CARTESIAN_POINT('Ctrl Pts',(33.988787154964,22.6827344516939,51.1497750043391));
#16205=CARTESIAN_POINT('Ctrl Pts',(34.0049582948499,22.6389806710746,51.1947768017134));
#16206=CARTESIAN_POINT('Ctrl Pts',(34.0180435398556,22.6017210834816,51.2498576675305));
#16207=CARTESIAN_POINT('Ctrl Pts',(34.035173686233,22.5520157275868,51.3712699229884));
#16208=CARTESIAN_POINT('Ctrl Pts',(34.0392910466663,22.5395928638606,51.4376004544113));
#16209=CARTESIAN_POINT('Ctrl Pts',(34.0392910466663,22.5395928638606,51.5623995455887));
#16210=CARTESIAN_POINT('Ctrl Pts',(34.035173686233,22.5520157275868,51.6287300770116));
#16211=CARTESIAN_POINT('Ctrl Pts',(34.0180435398556,22.6017210834816,51.7501423324695));
#16212=CARTESIAN_POINT('Ctrl Pts',(34.0049582948499,22.6389806710746,51.8052231982866));
#16213=CARTESIAN_POINT('Ctrl Pts',(33.9723690346461,22.7271564800506,51.8959141016255));
#16214=CARTESIAN_POINT('Ctrl Pts',(33.9500814962454,22.7852096676192,51.9357615493743));
#16215=CARTESIAN_POINT('Ctrl Pts',(33.8986190776695,22.9104700099307,51.9877768144645));
#16216=CARTESIAN_POINT('Ctrl Pts',(33.8693826555337,22.9776288701721,52.));
#16217=CARTESIAN_POINT('Ctrl Pts',(33.8408406745439,23.0395928638606,52.));
#16218=CARTESIAN_POINT('',(31.79383017385,25.2811069490433,48.5513791336308));
#16219=CARTESIAN_POINT('Origin',(29.2994615223724,20.9477335482704,52.8847525344037));
#16220=CARTESIAN_POINT('',(32.3261813122727,24.92755355845,47.6978257430375));
#16221=CARTESIAN_POINT('Ctrl Pts',(32.3261813122727,24.92755355845,47.6978257430375));
#16222=CARTESIAN_POINT('Ctrl Pts',(32.2311086046043,24.9998579453427,47.6978257430375));
#16223=CARTESIAN_POINT('Ctrl Pts',(32.1253144474337,25.0744920557659,47.7140189797529));
#16224=CARTESIAN_POINT('Ctrl Pts',(31.9158788492386,25.2103549049237,47.7786797574698));
#16225=CARTESIAN_POINT('Ctrl Pts',(31.812115448829,25.2717240182291,47.8264553384537));
#16226=CARTESIAN_POINT('Ctrl Pts',(31.6740901805616,25.348221870878,47.9239881120561));
#16227=CARTESIAN_POINT('Ctrl Pts',(31.6233390280396,25.3750874905218,47.9680392894922));
#16228=CARTESIAN_POINT('Ctrl Pts',(31.5656077205711,25.4047562084472,48.0459951427578));
#16229=CARTESIAN_POINT('Ctrl Pts',(31.5494384204252,25.4129061770103,48.0739431957104));
#16230=CARTESIAN_POINT('Ctrl Pts',(31.5266830274399,25.4242998143135,48.1333421546345));
#16231=CARTESIAN_POINT('Ctrl Pts',(31.5200949176888,25.42755355845,48.1647903548472));
#16232=CARTESIAN_POINT('Ctrl Pts',(31.5200949176888,25.42755355845,48.1978257430375));
#16233=CARTESIAN_POINT('Ctrl Pts',(31.5200949176888,25.42755355845,48.2308611312278));
#16234=CARTESIAN_POINT('Ctrl Pts',(31.5266830274399,25.4242998143135,48.2623093314405));
#16235=CARTESIAN_POINT('Ctrl Pts',(31.5494384204251,25.4129061770103,48.3217082903646));
#16236=CARTESIAN_POINT('Ctrl Pts',(31.5656077205711,25.4047562084472,48.3496563433172));
#16237=CARTESIAN_POINT('Ctrl Pts',(31.6233390280396,25.3750874905218,48.4276121965828));
#16238=CARTESIAN_POINT('Ctrl Pts',(31.6740901805616,25.348221870878,48.4716633740189));
#16239=CARTESIAN_POINT('Ctrl Pts',(31.7458731531068,25.3084375377237,48.522387364616));
#16240=CARTESIAN_POINT('Ctrl Pts',(31.7694876094241,25.2951189724682,48.5373671102059));
#16241=CARTESIAN_POINT('Ctrl Pts',(31.79383017385,25.2811069490433,48.5513791336308));
#16242=CARTESIAN_POINT('Origin',(29.2994615223724,20.9477335482704,47.6978257430375));
#16243=CARTESIAN_POINT('Origin',(71.2994615223724,-45.9821613702938,64.));
#16244=CARTESIAN_POINT('',(83.7994615223724,-45.9821613702938,64.));
#16245=CARTESIAN_POINT('Origin',(71.2994615223724,-45.9821613702938,64.));
#16246=CARTESIAN_POINT('',(83.7994615223724,-45.9821613702938,52.));
#16247=CARTESIAN_POINT('',(83.7994615223724,-45.9821613702938,64.));
#16248=CARTESIAN_POINT('',(58.8166289045012,-45.3272645584125,52.));
#16249=CARTESIAN_POINT('Origin',(71.2994615223724,-45.9821613702938,52.));
#16250=CARTESIAN_POINT('',(58.8529273319278,-44.8272645584125,51.5));
#16251=CARTESIAN_POINT('Ctrl Pts',(58.8529273319278,-44.8272645584125,51.5));
#16252=CARTESIAN_POINT('Ctrl Pts',(58.8529273319278,-44.8272645584125,51.5628289407498));
#16253=CARTESIAN_POINT('Ctrl Pts',(58.8517413197398,-44.83983109791,51.6298216562663));
#16254=CARTESIAN_POINT('Ctrl Pts',(58.847162227239,-44.8908782000976,51.7530059059081));
#16255=CARTESIAN_POINT('Ctrl Pts',(58.843796823021,-44.9293569823108,51.8091992050848));
#16256=CARTESIAN_POINT('Ctrl Pts',(58.8366132516778,-45.0181089553366,51.8979511781107));
#16257=CARTESIAN_POINT('Ctrl Pts',(58.8323191872735,-45.0743219277052,51.936421701237));
#16258=CARTESIAN_POINT('Ctrl Pts',(58.8239610728064,-45.1974964800649,51.9874465324277));
#16259=CARTESIAN_POINT('Ctrl Pts',(58.8199238582361,-45.264460227701,52.));
#16260=CARTESIAN_POINT('Ctrl Pts',(58.8166289045012,-45.3272645584125,52.));
#16261=CARTESIAN_POINT('',(58.8529273319278,-44.8272645584125,48.1978257430375));
#16262=CARTESIAN_POINT('',(58.8529273319278,-44.8272645584125,64.));
#16263=CARTESIAN_POINT('Ctrl Pts',(58.9094931389573,-44.3272645584125,47.6978257430375));
#16264=CARTESIAN_POINT('Ctrl Pts',(58.9011336612411,-44.3898507353038,47.6978257430375));
#16265=CARTESIAN_POINT('Ctrl Pts',(58.8927334019429,-44.4567282803349,47.7102969796753));
#16266=CARTESIAN_POINT('Ctrl Pts',(58.8782032929536,-44.5799514130651,47.7612544377797));
#16267=CARTESIAN_POINT('Ctrl Pts',(58.872046708812,-44.636291625979,47.7997460294175));
#16268=CARTESIAN_POINT('Ctrl Pts',(58.8627467322493,-44.7251367458781,47.8885911493166));
#16269=CARTESIAN_POINT('Ctrl Pts',(58.8589701728764,-44.7636241839714,47.9447717029639));
#16270=CARTESIAN_POINT('Ctrl Pts',(58.8540741990285,-44.8146887744293,48.0679654140368));
#16271=CARTESIAN_POINT('Ctrl Pts',(58.8529273319278,-44.8272645584125,48.1349780461073));
#16272=CARTESIAN_POINT('Ctrl Pts',(58.8529273319278,-44.8272645584125,48.1978257430375));
#16273=CARTESIAN_POINT('',(83.745995712817,-44.8272645584125,48.1978257430375));
#16274=CARTESIAN_POINT('Ctrl Pts',(83.745995712817,-44.8272645584125,48.1978257430375));
#16275=CARTESIAN_POINT('Ctrl Pts',(83.745995712817,-44.8272645584125,48.1349780461073));
#16276=CARTESIAN_POINT('Ctrl Pts',(83.7448488457163,-44.8146887744293,48.0679654140368));
#16277=CARTESIAN_POINT('Ctrl Pts',(83.7399528718684,-44.7636241839714,47.9447717029639));
#16278=CARTESIAN_POINT('Ctrl Pts',(83.7361763124955,-44.7251367458782,47.8885911493166));
#16279=CARTESIAN_POINT('Ctrl Pts',(83.7268763359328,-44.636291625979,47.7997460294175));
#16280=CARTESIAN_POINT('Ctrl Pts',(83.7207197517911,-44.5799514130651,47.7612544377797));
#16281=CARTESIAN_POINT('Ctrl Pts',(83.7061896428019,-44.4567282803349,47.7102969796753));
#16282=CARTESIAN_POINT('Ctrl Pts',(83.6977893835036,-44.3898507353038,47.6978257430375));
#16283=CARTESIAN_POINT('Ctrl Pts',(83.6894299057875,-44.3272645584125,47.6978257430375));
#16284=CARTESIAN_POINT('',(83.745995712817,-44.8272645584125,51.5));
#16285=CARTESIAN_POINT('',(83.745995712817,-44.8272645584125,64.));
#16286=CARTESIAN_POINT('',(83.7822941402435,-45.3272645584125,52.));
#16287=CARTESIAN_POINT('Ctrl Pts',(83.7822941402435,-45.3272645584125,52.));
#16288=CARTESIAN_POINT('Ctrl Pts',(83.7789991865087,-45.264460227701,52.));
#16289=CARTESIAN_POINT('Ctrl Pts',(83.7749619719384,-45.1974964800649,51.9874465324277));
#16290=CARTESIAN_POINT('Ctrl Pts',(83.7666038574713,-45.0743219277052,51.936421701237));
#16291=CARTESIAN_POINT('Ctrl Pts',(83.762309793067,-45.0181089553366,51.8979511781107));
#16292=CARTESIAN_POINT('Ctrl Pts',(83.7551262217237,-44.9293569823108,51.8091992050848));
#16293=CARTESIAN_POINT('Ctrl Pts',(83.7517608175058,-44.8908782000976,51.7530059059081));
#16294=CARTESIAN_POINT('Ctrl Pts',(83.747181725005,-44.83983109791,51.6298216562663));
#16295=CARTESIAN_POINT('Ctrl Pts',(83.745995712817,-44.8272645584125,51.5628289407498));
#16296=CARTESIAN_POINT('Ctrl Pts',(83.745995712817,-44.8272645584125,51.5));
#16297=CARTESIAN_POINT('Origin',(71.2994615223724,-45.9821613702938,52.));
#16298=CARTESIAN_POINT('Origin',(71.2994615223724,20.9477335482704,64.));
#16299=CARTESIAN_POINT('',(76.2994615223724,20.9477335482704,64.));
#16300=CARTESIAN_POINT('Origin',(71.2994615223724,20.9477335482704,64.));
#16301=CARTESIAN_POINT('',(76.2994615223724,20.9477335482704,47.6978257430375));
#16302=CARTESIAN_POINT('',(76.2994615223724,20.9477335482704,64.));
#16303=CARTESIAN_POINT('',(76.0987510891795,19.545300072509,47.6978257430375));
#16304=CARTESIAN_POINT('Origin',(71.2994615223724,20.9477335482704,47.6978257430375));
#16305=CARTESIAN_POINT('',(75.9233934931417,19.045300072509,47.1978257430375));
#16306=CARTESIAN_POINT('Ctrl Pts',(75.9233934931417,19.045300072509,47.1978257430375));
#16307=CARTESIAN_POINT('Ctrl Pts',(75.9233934931417,19.045300072509,47.2606262015597));
#16308=CARTESIAN_POINT('Ctrl Pts',(75.9286235220756,19.0578693331568,47.3272049658121));
#16309=CARTESIAN_POINT('Ctrl Pts',(75.9487439245958,19.1079235845375,47.4488825757172));
#16310=CARTESIAN_POINT('Ctrl Pts',(75.9635333627505,19.1453760973014,47.50401144732));
#16311=CARTESIAN_POINT('Ctrl Pts',(75.9963894622215,19.2327496876229,47.5933468507728));
#16312=CARTESIAN_POINT('Ctrl Pts',(76.0169336674919,19.2894923661088,47.6326971370671));
#16313=CARTESIAN_POINT('Ctrl Pts',(76.0588328495999,19.4138848506455,47.6849404681153));
#16314=CARTESIAN_POINT('Ctrl Pts',(76.0801249019844,19.4815591055255,47.6978257430375));
#16315=CARTESIAN_POINT('Ctrl Pts',(76.0987510891795,19.545300072509,47.6978257430375));
#16316=CARTESIAN_POINT('',(75.9233934931417,19.045300072509,36.1978257430375));
#16317=CARTESIAN_POINT('',(75.9233934931417,19.045300072509,64.));
#16318=CARTESIAN_POINT('',(75.6844716015559,18.545300072509,35.6978257430375));
#16319=CARTESIAN_POINT('Ctrl Pts',(75.6844716015559,18.545300072509,35.6978257430375));
#16320=CARTESIAN_POINT('Ctrl Pts',(75.7183437123576,18.6071246969023,35.6978257430375));
#16321=CARTESIAN_POINT('Ctrl Pts',(75.7533284422121,18.6744087742691,35.7099831569546));
#16322=CARTESIAN_POINT('Ctrl Pts',(75.8154443123393,18.800447936422,35.7624419799854));
#16323=CARTESIAN_POINT('Ctrl Pts',(75.8426335478405,18.8591453590194,35.8028130850757));
#16324=CARTESIAN_POINT('Ctrl Pts',(75.8819451449858,18.9470131641942,35.8942412268742));
#16325=CARTESIAN_POINT('Ctrl Pts',(75.8976695801488,18.983759545124,35.9488335262825));
#16326=CARTESIAN_POINT('Ctrl Pts',(75.9183580123699,19.0329211748031,36.0694921472959));
#16327=CARTESIAN_POINT('Ctrl Pts',(75.9233934931417,19.045300072509,36.1355610097978));
#16328=CARTESIAN_POINT('Ctrl Pts',(75.9233934931417,19.045300072509,36.1978257430375));
#16329=CARTESIAN_POINT('',(66.9144514431889,18.545300072509,35.6978257430375));
#16330=CARTESIAN_POINT('Origin',(71.2994615223724,20.9477335482704,35.6978257430375));
#16331=CARTESIAN_POINT('',(66.6755295516031,19.045300072509,36.1978257430375));
#16332=CARTESIAN_POINT('Ctrl Pts',(66.6755295516031,19.045300072509,36.1978257430375));
#16333=CARTESIAN_POINT('Ctrl Pts',(66.6755295516031,19.045300072509,36.1355610097978));
#16334=CARTESIAN_POINT('Ctrl Pts',(66.6805650323748,19.0329211748031,36.0694921472959));
#16335=CARTESIAN_POINT('Ctrl Pts',(66.701253464596,18.983759545124,35.9488335262825));
#16336=CARTESIAN_POINT('Ctrl Pts',(66.716977899759,18.9470131641942,35.8942412268742));
#16337=CARTESIAN_POINT('Ctrl Pts',(66.7562894969043,18.8591453590194,35.8028130850757));
#16338=CARTESIAN_POINT('Ctrl Pts',(66.7834787324055,18.800447936422,35.7624419799854));
#16339=CARTESIAN_POINT('Ctrl Pts',(66.8455946025327,18.6744087742692,35.7099831569546));
#16340=CARTESIAN_POINT('Ctrl Pts',(66.8805793323872,18.6071246969023,35.6978257430375));
#16341=CARTESIAN_POINT('Ctrl Pts',(66.9144514431889,18.545300072509,35.6978257430375));
#16342=CARTESIAN_POINT('',(66.6755295516031,19.045300072509,47.1978257430375));
#16343=CARTESIAN_POINT('',(66.6755295516031,19.045300072509,64.));
#16344=CARTESIAN_POINT('',(66.5001719555652,19.545300072509,47.6978257430375));
#16345=CARTESIAN_POINT('Ctrl Pts',(66.5001719555652,19.545300072509,47.6978257430375));
#16346=CARTESIAN_POINT('Ctrl Pts',(66.5187981427604,19.4815591055255,47.6978257430375));
#16347=CARTESIAN_POINT('Ctrl Pts',(66.5400901951449,19.4138848506455,47.6849404681153));
#16348=CARTESIAN_POINT('Ctrl Pts',(66.5819893772529,19.2894923661088,47.6326971370671));
#16349=CARTESIAN_POINT('Ctrl Pts',(66.6025335825233,19.2327496876229,47.5933468507728));
#16350=CARTESIAN_POINT('Ctrl Pts',(66.6353896819943,19.1453760973014,47.50401144732));
#16351=CARTESIAN_POINT('Ctrl Pts',(66.6501791201489,19.1079235845375,47.4488825757172));
#16352=CARTESIAN_POINT('Ctrl Pts',(66.6702995226691,19.0578693331568,47.3272049658121));
#16353=CARTESIAN_POINT('Ctrl Pts',(66.6755295516031,19.045300072509,47.2606262015597));
#16354=CARTESIAN_POINT('Ctrl Pts',(66.6755295516031,19.045300072509,47.1978257430375));
#16355=CARTESIAN_POINT('',(68.2727417324721,24.92755355845,47.6978257430375));
#16356=CARTESIAN_POINT('Origin',(71.2994615223724,20.9477335482704,47.6978257430375));
#16357=CARTESIAN_POINT('',(68.8050928708948,25.2811069490433,48.5513791336308));
#16358=CARTESIAN_POINT('Ctrl Pts',(68.8050928708948,25.2811069490433,48.5513791336308));
#16359=CARTESIAN_POINT('Ctrl Pts',(68.8294354351799,25.2951189723872,48.5373671102869));
#16360=CARTESIAN_POINT('Ctrl Pts',(68.8530498914273,25.308437537607,48.5223873647648));
#16361=CARTESIAN_POINT('Ctrl Pts',(68.9248328641831,25.348221870878,48.4716633740189));
#16362=CARTESIAN_POINT('Ctrl Pts',(68.9755840167052,25.3750874905218,48.4276121965828));
#16363=CARTESIAN_POINT('Ctrl Pts',(69.0333153241737,25.4047562084472,48.3496563433172));
#16364=CARTESIAN_POINT('Ctrl Pts',(69.0494846243196,25.4129061770103,48.3217082903646));
#16365=CARTESIAN_POINT('Ctrl Pts',(69.0722400173048,25.4242998143135,48.2623093314405));
#16366=CARTESIAN_POINT('Ctrl Pts',(69.078828127056,25.42755355845,48.2308611312278));
#16367=CARTESIAN_POINT('Ctrl Pts',(69.078828127056,25.42755355845,48.1978257430375));
#16368=CARTESIAN_POINT('Ctrl Pts',(69.078828127056,25.42755355845,48.1647903548472));
#16369=CARTESIAN_POINT('Ctrl Pts',(69.0722400173048,25.4242998143135,48.1333421546345));
#16370=CARTESIAN_POINT('Ctrl Pts',(69.0494846243196,25.4129061770103,48.0739431957104));
#16371=CARTESIAN_POINT('Ctrl Pts',(69.0333153241737,25.4047562084472,48.0459951427578));
#16372=CARTESIAN_POINT('Ctrl Pts',(68.9755840167052,25.3750874905218,47.9680392894922));
#16373=CARTESIAN_POINT('Ctrl Pts',(68.9248328641831,25.348221870878,47.9239881120561));
#16374=CARTESIAN_POINT('Ctrl Pts',(68.7868075959158,25.2717240182291,47.8264553384537));
#16375=CARTESIAN_POINT('Ctrl Pts',(68.6830441955061,25.2103549049236,47.7786797574698));
#16376=CARTESIAN_POINT('Ctrl Pts',(68.4736085973111,25.0744920557659,47.7140189797529));
#16377=CARTESIAN_POINT('Ctrl Pts',(68.3678144401405,24.9998579453427,47.6978257430375));
#16378=CARTESIAN_POINT('Ctrl Pts',(68.2727417324721,24.92755355845,47.6978257430375));
#16379=CARTESIAN_POINT('',(66.6113603597352,22.6860394732673,51.1464466094067));
#16380=CARTESIAN_POINT('Origin',(71.2994615223724,20.9477335482704,52.8847525344037));
#16381=CARTESIAN_POINT('',(66.7580823702008,23.0395928638606,52.));
#16382=CARTESIAN_POINT('Ctrl Pts',(66.7580823702008,23.0395928638606,52.));
#16383=CARTESIAN_POINT('Ctrl Pts',(66.7295403892111,22.9776288701721,52.));
#16384=CARTESIAN_POINT('Ctrl Pts',(66.7003039670752,22.9104700099307,51.9877768144645));
#16385=CARTESIAN_POINT('Ctrl Pts',(66.6488415484994,22.7852096676192,51.9357615493743));
#16386=CARTESIAN_POINT('Ctrl Pts',(66.6265540100987,22.7271564800506,51.8959141016255));
#16387=CARTESIAN_POINT('Ctrl Pts',(66.5939647498949,22.6389806710746,51.8052231982866));
#16388=CARTESIAN_POINT('Ctrl Pts',(66.5808795048891,22.6017210834815,51.7501423324695));
#16389=CARTESIAN_POINT('Ctrl Pts',(66.5637493585117,22.5520157275868,51.6287300770116));
#16390=CARTESIAN_POINT('Ctrl Pts',(66.5596319980784,22.5395928638606,51.5623995455887));
#16391=CARTESIAN_POINT('Ctrl Pts',(66.5596319980784,22.5395928638606,51.4376004544113));
#16392=CARTESIAN_POINT('Ctrl Pts',(66.5637493585117,22.5520157275868,51.3712699229884));
#16393=CARTESIAN_POINT('Ctrl Pts',(66.5808795048891,22.6017210834815,51.2498576675305));
#16394=CARTESIAN_POINT('Ctrl Pts',(66.5939647498949,22.6389806710746,51.1947768017134));
#16395=CARTESIAN_POINT('Ctrl Pts',(66.6101358897808,22.6827344516939,51.1497750043391));
#16396=CARTESIAN_POINT('Ctrl Pts',(66.610744984223,22.6843798444226,51.1481062382515));
#16397=CARTESIAN_POINT('Ctrl Pts',(66.6113603597352,22.6860394732673,51.1464466094067));
#16398=CARTESIAN_POINT('',(75.840840674544,23.0395928638606,52.));
#16399=CARTESIAN_POINT('Origin',(71.2994615223724,20.9477335482704,52.));
#16400=CARTESIAN_POINT('',(75.9875626850096,22.6860394732673,51.1464466094067));
#16401=CARTESIAN_POINT('Ctrl Pts',(75.9875626850096,22.6860394732673,51.1464466094067));
#16402=CARTESIAN_POINT('Ctrl Pts',(75.9881780605218,22.6843798444226,51.1481062382515));
#16403=CARTESIAN_POINT('Ctrl Pts',(75.988787154964,22.6827344516939,51.1497750043391));
#16404=CARTESIAN_POINT('Ctrl Pts',(76.0049582948499,22.6389806710746,51.1947768017134));
#16405=CARTESIAN_POINT('Ctrl Pts',(76.0180435398557,22.6017210834815,51.2498576675305));
#16406=CARTESIAN_POINT('Ctrl Pts',(76.035173686233,22.5520157275867,51.3712699229885));
#16407=CARTESIAN_POINT('Ctrl Pts',(76.0392910466663,22.5395928638606,51.4376004544113));
#16408=CARTESIAN_POINT('Ctrl Pts',(76.0392910466663,22.5395928638606,51.5623995455887));
#16409=CARTESIAN_POINT('Ctrl Pts',(76.035173686233,22.5520157275868,51.6287300770116));
#16410=CARTESIAN_POINT('Ctrl Pts',(76.0180435398557,22.6017210834815,51.7501423324695));
#16411=CARTESIAN_POINT('Ctrl Pts',(76.0049582948499,22.6389806710746,51.8052231982866));
#16412=CARTESIAN_POINT('Ctrl Pts',(75.9723690346461,22.7271564800506,51.8959141016255));
#16413=CARTESIAN_POINT('Ctrl Pts',(75.9500814962454,22.7852096676192,51.9357615493743));
#16414=CARTESIAN_POINT('Ctrl Pts',(75.8986190776695,22.9104700099307,51.9877768144645));
#16415=CARTESIAN_POINT('Ctrl Pts',(75.8693826555337,22.9776288701721,52.));
#16416=CARTESIAN_POINT('Ctrl Pts',(75.840840674544,23.0395928638606,52.));
#16417=CARTESIAN_POINT('',(73.79383017385,25.2811069490433,48.5513791336308));
#16418=CARTESIAN_POINT('Origin',(71.2994615223724,20.9477335482704,52.8847525344037));
#16419=CARTESIAN_POINT('',(74.3261813122727,24.92755355845,47.6978257430375));
#16420=CARTESIAN_POINT('Ctrl Pts',(74.3261813122727,24.92755355845,47.6978257430375));
#16421=CARTESIAN_POINT('Ctrl Pts',(74.2311086046043,24.9998579453427,47.6978257430375));
#16422=CARTESIAN_POINT('Ctrl Pts',(74.1253144474337,25.0744920557659,47.7140189797529));
#16423=CARTESIAN_POINT('Ctrl Pts',(73.9158788492387,25.2103549049236,47.7786797574698));
#16424=CARTESIAN_POINT('Ctrl Pts',(73.812115448829,25.2717240182291,47.8264553384537));
#16425=CARTESIAN_POINT('Ctrl Pts',(73.6740901805616,25.348221870878,47.9239881120561));
#16426=CARTESIAN_POINT('Ctrl Pts',(73.6233390280396,25.3750874905218,47.9680392894922));
#16427=CARTESIAN_POINT('Ctrl Pts',(73.5656077205711,25.4047562084472,48.0459951427578));
#16428=CARTESIAN_POINT('Ctrl Pts',(73.5494384204252,25.4129061770103,48.0739431957104));
#16429=CARTESIAN_POINT('Ctrl Pts',(73.52668302744,25.4242998143135,48.1333421546345));
#16430=CARTESIAN_POINT('Ctrl Pts',(73.5200949176888,25.42755355845,48.1647903548472));
#16431=CARTESIAN_POINT('Ctrl Pts',(73.5200949176888,25.42755355845,48.1978257430375));
#16432=CARTESIAN_POINT('Ctrl Pts',(73.5200949176888,25.42755355845,48.2308611312278));
#16433=CARTESIAN_POINT('Ctrl Pts',(73.5266830274399,25.4242998143135,48.2623093314405));
#16434=CARTESIAN_POINT('Ctrl Pts',(73.5494384204251,25.4129061770103,48.3217082903646));
#16435=CARTESIAN_POINT('Ctrl Pts',(73.5656077205711,25.4047562084472,48.3496563433172));
#16436=CARTESIAN_POINT('Ctrl Pts',(73.6233390280396,25.3750874905218,48.4276121965828));
#16437=CARTESIAN_POINT('Ctrl Pts',(73.6740901805616,25.348221870878,48.4716633740189));
#16438=CARTESIAN_POINT('Ctrl Pts',(73.7458731531068,25.3084375377237,48.522387364616));
#16439=CARTESIAN_POINT('Ctrl Pts',(73.7694876094241,25.2951189724682,48.5373671102059));
#16440=CARTESIAN_POINT('Ctrl Pts',(73.79383017385,25.2811069490433,48.5513791336308));
#16441=CARTESIAN_POINT('Origin',(71.2994615223724,20.9477335482704,47.6978257430375));
#16442=CARTESIAN_POINT('Origin',(-12.7005384776276,20.9477335482704,64.));
#16443=CARTESIAN_POINT('',(-7.70053847762761,20.9477335482704,64.));
#16444=CARTESIAN_POINT('Origin',(-12.7005384776276,20.9477335482704,64.));
#16445=CARTESIAN_POINT('',(-7.70053847762761,20.9477335482704,47.6978257430375));
#16446=CARTESIAN_POINT('',(-7.70053847762761,20.9477335482704,64.));
#16447=CARTESIAN_POINT('',(-7.90124891082047,19.545300072509,47.6978257430375));
#16448=CARTESIAN_POINT('Origin',(-12.7005384776276,20.9477335482704,47.6978257430375));
#16449=CARTESIAN_POINT('',(-8.0766065068583,19.045300072509,47.1978257430375));
#16450=CARTESIAN_POINT('Ctrl Pts',(-8.0766065068583,19.045300072509,47.1978257430375));
#16451=CARTESIAN_POINT('Ctrl Pts',(-8.0766065068583,19.045300072509,47.2606262015597));
#16452=CARTESIAN_POINT('Ctrl Pts',(-8.07137647792435,19.0578693331568,47.3272049658121));
#16453=CARTESIAN_POINT('Ctrl Pts',(-8.05125607540415,19.1079235845375,47.4488825757172));
#16454=CARTESIAN_POINT('Ctrl Pts',(-8.03646663724948,19.1453760973014,47.50401144732));
#16455=CARTESIAN_POINT('Ctrl Pts',(-8.00361053777846,19.2327496876229,47.5933468507728));
#16456=CARTESIAN_POINT('Ctrl Pts',(-7.98306633250816,19.2894923661088,47.6326971370671));
#16457=CARTESIAN_POINT('Ctrl Pts',(-7.94116715040014,19.4138848506455,47.6849404681153));
#16458=CARTESIAN_POINT('Ctrl Pts',(-7.91987509801561,19.4815591055256,47.6978257430375));
#16459=CARTESIAN_POINT('Ctrl Pts',(-7.90124891082047,19.545300072509,47.6978257430375));
#16460=CARTESIAN_POINT('',(-8.0766065068583,19.045300072509,36.1978257430375));
#16461=CARTESIAN_POINT('',(-8.0766065068583,19.045300072509,64.));
#16462=CARTESIAN_POINT('',(-8.31552839844407,18.545300072509,35.6978257430375));
#16463=CARTESIAN_POINT('Ctrl Pts',(-8.31552839844407,18.545300072509,35.6978257430375));
#16464=CARTESIAN_POINT('Ctrl Pts',(-8.28165628764236,18.6071246969023,35.6978257430375));
#16465=CARTESIAN_POINT('Ctrl Pts',(-8.24667155778788,18.6744087742692,35.7099831569546));
#16466=CARTESIAN_POINT('Ctrl Pts',(-8.18455568766068,18.800447936422,35.7624419799854));
#16467=CARTESIAN_POINT('Ctrl Pts',(-8.15736645215949,18.8591453590194,35.8028130850757));
#16468=CARTESIAN_POINT('Ctrl Pts',(-8.11805485501417,18.9470131641943,35.8942412268742));
#16469=CARTESIAN_POINT('Ctrl Pts',(-8.10233041985118,18.983759545124,35.9488335262825));
#16470=CARTESIAN_POINT('Ctrl Pts',(-8.08164198763004,19.0329211748031,36.0694921472959));
#16471=CARTESIAN_POINT('Ctrl Pts',(-8.0766065068583,19.045300072509,36.1355610097978));
#16472=CARTESIAN_POINT('Ctrl Pts',(-8.0766065068583,19.045300072509,36.1978257430375));
#16473=CARTESIAN_POINT('',(-17.0855485568112,18.545300072509,35.6978257430375));
#16474=CARTESIAN_POINT('Origin',(-12.7005384776276,20.9477335482704,35.6978257430375));
#16475=CARTESIAN_POINT('',(-17.3244704483969,19.045300072509,36.1978257430375));
#16476=CARTESIAN_POINT('Ctrl Pts',(-17.3244704483969,19.045300072509,36.1978257430375));
#16477=CARTESIAN_POINT('Ctrl Pts',(-17.3244704483969,19.045300072509,36.1355610097978));
#16478=CARTESIAN_POINT('Ctrl Pts',(-17.3194349676252,19.0329211748031,36.0694921472959));
#16479=CARTESIAN_POINT('Ctrl Pts',(-17.298746535404,18.983759545124,35.9488335262825));
#16480=CARTESIAN_POINT('Ctrl Pts',(-17.2830221002411,18.9470131641943,35.8942412268742));
#16481=CARTESIAN_POINT('Ctrl Pts',(-17.2437105030957,18.8591453590194,35.8028130850757));
#16482=CARTESIAN_POINT('Ctrl Pts',(-17.2165212675945,18.800447936422,35.7624419799854));
#16483=CARTESIAN_POINT('Ctrl Pts',(-17.1544053974673,18.6744087742692,35.7099831569546));
#16484=CARTESIAN_POINT('Ctrl Pts',(-17.1194206676129,18.6071246969023,35.6978257430375));
#16485=CARTESIAN_POINT('Ctrl Pts',(-17.0855485568111,18.545300072509,35.6978257430375));
#16486=CARTESIAN_POINT('',(-17.3244704483969,19.045300072509,47.1978257430375));
#16487=CARTESIAN_POINT('',(-17.3244704483969,19.045300072509,64.));
#16488=CARTESIAN_POINT('',(-17.4998280444348,19.545300072509,47.6978257430375));
#16489=CARTESIAN_POINT('Ctrl Pts',(-17.4998280444348,19.545300072509,47.6978257430375));
#16490=CARTESIAN_POINT('Ctrl Pts',(-17.4812018572396,19.4815591055256,47.6978257430375));
#16491=CARTESIAN_POINT('Ctrl Pts',(-17.4599098048551,19.4138848506455,47.6849404681153));
#16492=CARTESIAN_POINT('Ctrl Pts',(-17.4180106227471,19.2894923661088,47.6326971370671));
#16493=CARTESIAN_POINT('Ctrl Pts',(-17.3974664174768,19.2327496876229,47.5933468507728));
#16494=CARTESIAN_POINT('Ctrl Pts',(-17.3646103180057,19.1453760973014,47.50401144732));
#16495=CARTESIAN_POINT('Ctrl Pts',(-17.3498208798511,19.1079235845375,47.4488825757172));
#16496=CARTESIAN_POINT('Ctrl Pts',(-17.3297004773309,19.0578693331568,47.3272049658121));
#16497=CARTESIAN_POINT('Ctrl Pts',(-17.3244704483969,19.045300072509,47.2606262015597));
#16498=CARTESIAN_POINT('Ctrl Pts',(-17.3244704483969,19.045300072509,47.1978257430375));
#16499=CARTESIAN_POINT('',(-15.7272582675279,24.92755355845,47.6978257430375));
#16500=CARTESIAN_POINT('Origin',(-12.7005384776276,20.9477335482704,47.6978257430375));
#16501=CARTESIAN_POINT('',(-15.1949071291052,25.2811069490433,48.5513791336308));
#16502=CARTESIAN_POINT('Ctrl Pts',(-15.1949071291052,25.2811069490433,48.5513791336308));
#16503=CARTESIAN_POINT('Ctrl Pts',(-15.17056456482,25.2951189723872,48.5373671102869));
#16504=CARTESIAN_POINT('Ctrl Pts',(-15.1469501085726,25.308437537607,48.5223873647648));
#16505=CARTESIAN_POINT('Ctrl Pts',(-15.0751671358168,25.348221870878,48.4716633740189));
#16506=CARTESIAN_POINT('Ctrl Pts',(-15.0244159832948,25.3750874905218,48.4276121965828));
#16507=CARTESIAN_POINT('Ctrl Pts',(-14.9666846758263,25.4047562084472,48.3496563433172));
#16508=CARTESIAN_POINT('Ctrl Pts',(-14.9505153756804,25.4129061770103,48.3217082903646));
#16509=CARTESIAN_POINT('Ctrl Pts',(-14.9277599826951,25.4242998143135,48.2623093314405));
#16510=CARTESIAN_POINT('Ctrl Pts',(-14.921171872944,25.42755355845,48.2308611312278));
#16511=CARTESIAN_POINT('Ctrl Pts',(-14.921171872944,25.42755355845,48.1978257430375));
#16512=CARTESIAN_POINT('Ctrl Pts',(-14.921171872944,25.42755355845,48.1647903548472));
#16513=CARTESIAN_POINT('Ctrl Pts',(-14.9277599826951,25.4242998143135,48.1333421546345));
#16514=CARTESIAN_POINT('Ctrl Pts',(-14.9505153756804,25.4129061770103,48.0739431957104));
#16515=CARTESIAN_POINT('Ctrl Pts',(-14.9666846758263,25.4047562084472,48.0459951427578));
#16516=CARTESIAN_POINT('Ctrl Pts',(-15.0244159832948,25.3750874905218,47.9680392894922));
#16517=CARTESIAN_POINT('Ctrl Pts',(-15.0751671358168,25.348221870878,47.9239881120561));
#16518=CARTESIAN_POINT('Ctrl Pts',(-15.2131924040842,25.2717240182291,47.8264553384537));
#16519=CARTESIAN_POINT('Ctrl Pts',(-15.3169558044939,25.2103549049237,47.7786797574698));
#16520=CARTESIAN_POINT('Ctrl Pts',(-15.5263914026889,25.0744920557659,47.7140189797529));
#16521=CARTESIAN_POINT('Ctrl Pts',(-15.6321855598595,24.9998579453427,47.6978257430375));
#16522=CARTESIAN_POINT('Ctrl Pts',(-15.7272582675279,24.92755355845,47.6978257430375));
#16523=CARTESIAN_POINT('',(-17.3886396402648,22.6860394732673,51.1464466094067));
#16524=CARTESIAN_POINT('Origin',(-12.7005384776276,20.9477335482704,52.8847525344037));
#16525=CARTESIAN_POINT('',(-17.2419176297992,23.0395928638606,52.));
#16526=CARTESIAN_POINT('Ctrl Pts',(-17.2419176297992,23.0395928638606,52.));
#16527=CARTESIAN_POINT('Ctrl Pts',(-17.2704596107889,22.9776288701721,52.));
#16528=CARTESIAN_POINT('Ctrl Pts',(-17.2996960329247,22.9104700099307,51.9877768144645));
#16529=CARTESIAN_POINT('Ctrl Pts',(-17.3511584515006,22.7852096676192,51.9357615493743));
#16530=CARTESIAN_POINT('Ctrl Pts',(-17.3734459899013,22.7271564800506,51.8959141016255));
#16531=CARTESIAN_POINT('Ctrl Pts',(-17.4060352501051,22.6389806710746,51.8052231982866));
#16532=CARTESIAN_POINT('Ctrl Pts',(-17.4191204951109,22.6017210834816,51.7501423324695));
#16533=CARTESIAN_POINT('Ctrl Pts',(-17.4362506414882,22.5520157275868,51.6287300770116));
#16534=CARTESIAN_POINT('Ctrl Pts',(-17.4403680019216,22.5395928638606,51.5623995455887));
#16535=CARTESIAN_POINT('Ctrl Pts',(-17.4403680019216,22.5395928638606,51.4376004544113));
#16536=CARTESIAN_POINT('Ctrl Pts',(-17.4362506414882,22.5520157275868,51.3712699229884));
#16537=CARTESIAN_POINT('Ctrl Pts',(-17.4191204951109,22.6017210834816,51.2498576675305));
#16538=CARTESIAN_POINT('Ctrl Pts',(-17.4060352501051,22.6389806710746,51.1947768017134));
#16539=CARTESIAN_POINT('Ctrl Pts',(-17.3898641102192,22.682734451694,51.1497750043391));
#16540=CARTESIAN_POINT('Ctrl Pts',(-17.389255015777,22.6843798444226,51.1481062382515));
#16541=CARTESIAN_POINT('Ctrl Pts',(-17.3886396402648,22.6860394732673,51.1464466094067));
#16542=CARTESIAN_POINT('',(-8.15915932545606,23.0395928638606,52.));
#16543=CARTESIAN_POINT('Origin',(-12.7005384776276,20.9477335482704,52.));
#16544=CARTESIAN_POINT('',(-8.01243731499038,22.6860394732673,51.1464466094067));
#16545=CARTESIAN_POINT('Ctrl Pts',(-8.01243731499038,22.6860394732673,51.1464466094067));
#16546=CARTESIAN_POINT('Ctrl Pts',(-8.0118219394782,22.6843798444226,51.1481062382515));
#16547=CARTESIAN_POINT('Ctrl Pts',(-8.01121284503603,22.682734451694,51.1497750043391));
#16548=CARTESIAN_POINT('Ctrl Pts',(-7.99504170515014,22.6389806710746,51.1947768017134));
#16549=CARTESIAN_POINT('Ctrl Pts',(-7.98195646014436,22.6017210834816,51.2498576675305));
#16550=CARTESIAN_POINT('Ctrl Pts',(-7.96482631376698,22.5520157275868,51.3712699229884));
#16551=CARTESIAN_POINT('Ctrl Pts',(-7.96070895333366,22.5395928638606,51.4376004544113));
#16552=CARTESIAN_POINT('Ctrl Pts',(-7.96070895333366,22.5395928638606,51.5623995455887));
#16553=CARTESIAN_POINT('Ctrl Pts',(-7.96482631376698,22.5520157275868,51.6287300770116));
#16554=CARTESIAN_POINT('Ctrl Pts',(-7.98195646014436,22.6017210834816,51.7501423324695));
#16555=CARTESIAN_POINT('Ctrl Pts',(-7.99504170515014,22.6389806710746,51.8052231982866));
#16556=CARTESIAN_POINT('Ctrl Pts',(-8.02763096535394,22.7271564800506,51.8959141016255));
#16557=CARTESIAN_POINT('Ctrl Pts',(-8.04991850375465,22.7852096676192,51.9357615493743));
#16558=CARTESIAN_POINT('Ctrl Pts',(-8.10138092233047,22.9104700099307,51.9877768144645));
#16559=CARTESIAN_POINT('Ctrl Pts',(-8.13061734446632,22.9776288701721,52.));
#16560=CARTESIAN_POINT('Ctrl Pts',(-8.15915932545606,23.0395928638606,52.));
#16561=CARTESIAN_POINT('',(-10.2061698261501,25.2811069490433,48.5513791336308));
#16562=CARTESIAN_POINT('Origin',(-12.7005384776276,20.9477335482704,52.8847525344037));
#16563=CARTESIAN_POINT('',(-9.67381868772735,24.92755355845,47.6978257430375));
#16564=CARTESIAN_POINT('Ctrl Pts',(-9.67381868772736,24.92755355845,47.6978257430375));
#16565=CARTESIAN_POINT('Ctrl Pts',(-9.76889139539571,24.9998579453427,47.6978257430375));
#16566=CARTESIAN_POINT('Ctrl Pts',(-9.87468555256633,25.0744920557659,47.7140189797529));
#16567=CARTESIAN_POINT('Ctrl Pts',(-10.0841211507614,25.2103549049237,47.7786797574698));
#16568=CARTESIAN_POINT('Ctrl Pts',(-10.187884551171,25.2717240182291,47.8264553384537));
#16569=CARTESIAN_POINT('Ctrl Pts',(-10.3259098194384,25.348221870878,47.9239881120561));
#16570=CARTESIAN_POINT('Ctrl Pts',(-10.3766609719604,25.3750874905218,47.9680392894922));
#16571=CARTESIAN_POINT('Ctrl Pts',(-10.434392279429,25.4047562084472,48.0459951427578));
#16572=CARTESIAN_POINT('Ctrl Pts',(-10.4505615795749,25.4129061770103,48.0739431957104));
#16573=CARTESIAN_POINT('Ctrl Pts',(-10.4733169725601,25.4242998143135,48.1333421546345));
#16574=CARTESIAN_POINT('Ctrl Pts',(-10.4799050823113,25.42755355845,48.1647903548472));
#16575=CARTESIAN_POINT('Ctrl Pts',(-10.4799050823113,25.42755355845,48.1978257430375));
#16576=CARTESIAN_POINT('Ctrl Pts',(-10.4799050823113,25.42755355845,48.2308611312278));
#16577=CARTESIAN_POINT('Ctrl Pts',(-10.4733169725601,25.4242998143135,48.2623093314405));
#16578=CARTESIAN_POINT('Ctrl Pts',(-10.4505615795749,25.4129061770103,48.3217082903646));
#16579=CARTESIAN_POINT('Ctrl Pts',(-10.434392279429,25.4047562084472,48.3496563433172));
#16580=CARTESIAN_POINT('Ctrl Pts',(-10.3766609719604,25.3750874905218,48.4276121965828));
#16581=CARTESIAN_POINT('Ctrl Pts',(-10.3259098194384,25.348221870878,48.4716633740189));
#16582=CARTESIAN_POINT('Ctrl Pts',(-10.2541268468932,25.3084375377237,48.522387364616));
#16583=CARTESIAN_POINT('Ctrl Pts',(-10.2305123905759,25.2951189724682,48.5373671102059));
#16584=CARTESIAN_POINT('Ctrl Pts',(-10.2061698261501,25.2811069490433,48.5513791336308));
#16585=CARTESIAN_POINT('Origin',(-12.7005384776276,20.9477335482704,47.6978257430375));
#16586=CARTESIAN_POINT('Origin',(-54.7005384776276,20.9477335482704,64.));
#16587=CARTESIAN_POINT('',(-49.7005384776276,20.9477335482704,64.));
#16588=CARTESIAN_POINT('Origin',(-54.7005384776276,20.9477335482704,64.));
#16589=CARTESIAN_POINT('',(-49.7005384776276,20.9477335482704,47.6978257430375));
#16590=CARTESIAN_POINT('',(-49.7005384776276,20.9477335482704,64.));
#16591=CARTESIAN_POINT('',(-49.9012489108205,19.5453000725091,47.6978257430375));
#16592=CARTESIAN_POINT('Origin',(-54.7005384776276,20.9477335482704,47.6978257430375));
#16593=CARTESIAN_POINT('',(-50.0766065068583,19.0453000725091,47.1978257430375));
#16594=CARTESIAN_POINT('Ctrl Pts',(-50.0766065068583,19.0453000725091,47.1978257430375));
#16595=CARTESIAN_POINT('Ctrl Pts',(-50.0766065068583,19.0453000725091,47.2606262015597));
#16596=CARTESIAN_POINT('Ctrl Pts',(-50.0713764779243,19.0578693331568,47.3272049658121));
#16597=CARTESIAN_POINT('Ctrl Pts',(-50.0512560754041,19.1079235845375,47.4488825757172));
#16598=CARTESIAN_POINT('Ctrl Pts',(-50.0364666372495,19.1453760973015,47.50401144732));
#16599=CARTESIAN_POINT('Ctrl Pts',(-50.0036105377785,19.2327496876229,47.5933468507728));
#16600=CARTESIAN_POINT('Ctrl Pts',(-49.9830663325081,19.2894923661088,47.6326971370671));
#16601=CARTESIAN_POINT('Ctrl Pts',(-49.9411671504001,19.4138848506455,47.6849404681153));
#16602=CARTESIAN_POINT('Ctrl Pts',(-49.9198750980156,19.4815591055256,47.6978257430375));
#16603=CARTESIAN_POINT('Ctrl Pts',(-49.9012489108205,19.5453000725091,47.6978257430375));
#16604=CARTESIAN_POINT('',(-50.0766065068583,19.0453000725091,36.1978257430375));
#16605=CARTESIAN_POINT('',(-50.0766065068583,19.0453000725091,64.));
#16606=CARTESIAN_POINT('',(-50.3155283984441,18.5453000725091,35.6978257430375));
#16607=CARTESIAN_POINT('Ctrl Pts',(-50.3155283984441,18.5453000725091,35.6978257430375));
#16608=CARTESIAN_POINT('Ctrl Pts',(-50.2816562876424,18.6071246969023,35.6978257430375));
#16609=CARTESIAN_POINT('Ctrl Pts',(-50.2466715577879,18.6744087742692,35.7099831569546));
#16610=CARTESIAN_POINT('Ctrl Pts',(-50.1845556876607,18.800447936422,35.7624419799854));
#16611=CARTESIAN_POINT('Ctrl Pts',(-50.1573664521595,18.8591453590194,35.8028130850757));
#16612=CARTESIAN_POINT('Ctrl Pts',(-50.1180548550142,18.9470131641943,35.8942412268742));
#16613=CARTESIAN_POINT('Ctrl Pts',(-50.1023304198512,18.9837595451241,35.9488335262825));
#16614=CARTESIAN_POINT('Ctrl Pts',(-50.08164198763,19.0329211748031,36.0694921472959));
#16615=CARTESIAN_POINT('Ctrl Pts',(-50.0766065068583,19.0453000725091,36.1355610097978));
#16616=CARTESIAN_POINT('Ctrl Pts',(-50.0766065068583,19.0453000725091,36.1978257430375));
#16617=CARTESIAN_POINT('',(-59.0855485568112,18.5453000725091,35.6978257430375));
#16618=CARTESIAN_POINT('Origin',(-54.7005384776276,20.9477335482704,35.6978257430375));
#16619=CARTESIAN_POINT('',(-59.3244704483969,19.0453000725091,36.1978257430375));
#16620=CARTESIAN_POINT('Ctrl Pts',(-59.3244704483969,19.0453000725091,36.1978257430375));
#16621=CARTESIAN_POINT('Ctrl Pts',(-59.3244704483969,19.0453000725091,36.1355610097978));
#16622=CARTESIAN_POINT('Ctrl Pts',(-59.3194349676252,19.0329211748031,36.0694921472959));
#16623=CARTESIAN_POINT('Ctrl Pts',(-59.298746535404,18.9837595451241,35.9488335262825));
#16624=CARTESIAN_POINT('Ctrl Pts',(-59.2830221002411,18.9470131641943,35.8942412268742));
#16625=CARTESIAN_POINT('Ctrl Pts',(-59.2437105030957,18.8591453590194,35.8028130850757));
#16626=CARTESIAN_POINT('Ctrl Pts',(-59.2165212675946,18.800447936422,35.7624419799854));
#16627=CARTESIAN_POINT('Ctrl Pts',(-59.1544053974674,18.6744087742692,35.7099831569546));
#16628=CARTESIAN_POINT('Ctrl Pts',(-59.1194206676129,18.6071246969023,35.6978257430375));
#16629=CARTESIAN_POINT('Ctrl Pts',(-59.0855485568112,18.5453000725091,35.6978257430375));
#16630=CARTESIAN_POINT('',(-59.3244704483969,19.0453000725091,47.1978257430375));
#16631=CARTESIAN_POINT('',(-59.3244704483969,19.0453000725091,64.));
#16632=CARTESIAN_POINT('',(-59.4998280444348,19.5453000725091,47.6978257430375));
#16633=CARTESIAN_POINT('Ctrl Pts',(-59.4998280444348,19.5453000725091,47.6978257430375));
#16634=CARTESIAN_POINT('Ctrl Pts',(-59.4812018572396,19.4815591055256,47.6978257430375));
#16635=CARTESIAN_POINT('Ctrl Pts',(-59.4599098048551,19.4138848506455,47.6849404681153));
#16636=CARTESIAN_POINT('Ctrl Pts',(-59.4180106227471,19.2894923661088,47.6326971370671));
#16637=CARTESIAN_POINT('Ctrl Pts',(-59.3974664174768,19.2327496876229,47.5933468507728));
#16638=CARTESIAN_POINT('Ctrl Pts',(-59.3646103180058,19.1453760973015,47.50401144732));
#16639=CARTESIAN_POINT('Ctrl Pts',(-59.3498208798511,19.1079235845375,47.4488825757172));
#16640=CARTESIAN_POINT('Ctrl Pts',(-59.3297004773309,19.0578693331568,47.3272049658121));
#16641=CARTESIAN_POINT('Ctrl Pts',(-59.3244704483969,19.0453000725091,47.2606262015597));
#16642=CARTESIAN_POINT('Ctrl Pts',(-59.3244704483969,19.0453000725091,47.1978257430375));
#16643=CARTESIAN_POINT('',(-57.7272582675279,24.92755355845,47.6978257430375));
#16644=CARTESIAN_POINT('Origin',(-54.7005384776276,20.9477335482704,47.6978257430375));
#16645=CARTESIAN_POINT('',(-57.1949071291051,25.2811069490433,48.5513791336308));
#16646=CARTESIAN_POINT('Ctrl Pts',(-57.1949071291051,25.2811069490433,48.5513791336308));
#16647=CARTESIAN_POINT('Ctrl Pts',(-57.17056456482,25.2951189723872,48.5373671102869));
#16648=CARTESIAN_POINT('Ctrl Pts',(-57.1469501085726,25.308437537607,48.5223873647648));
#16649=CARTESIAN_POINT('Ctrl Pts',(-57.0751671358168,25.348221870878,48.4716633740189));
#16650=CARTESIAN_POINT('Ctrl Pts',(-57.0244159832948,25.3750874905218,48.4276121965828));
#16651=CARTESIAN_POINT('Ctrl Pts',(-56.9666846758262,25.4047562084472,48.3496563433172));
#16652=CARTESIAN_POINT('Ctrl Pts',(-56.9505153756803,25.4129061770103,48.3217082903646));
#16653=CARTESIAN_POINT('Ctrl Pts',(-56.9277599826951,25.4242998143135,48.2623093314405));
#16654=CARTESIAN_POINT('Ctrl Pts',(-56.9211718729439,25.42755355845,48.2308611312278));
#16655=CARTESIAN_POINT('Ctrl Pts',(-56.9211718729439,25.42755355845,48.1978257430375));
#16656=CARTESIAN_POINT('Ctrl Pts',(-56.9211718729439,25.42755355845,48.1647903548472));
#16657=CARTESIAN_POINT('Ctrl Pts',(-56.9277599826951,25.4242998143135,48.1333421546345));
#16658=CARTESIAN_POINT('Ctrl Pts',(-56.9505153756803,25.4129061770103,48.0739431957104));
#16659=CARTESIAN_POINT('Ctrl Pts',(-56.9666846758262,25.4047562084472,48.0459951427578));
#16660=CARTESIAN_POINT('Ctrl Pts',(-57.0244159832948,25.3750874905218,47.9680392894922));
#16661=CARTESIAN_POINT('Ctrl Pts',(-57.0751671358168,25.348221870878,47.9239881120561));
#16662=CARTESIAN_POINT('Ctrl Pts',(-57.2131924040842,25.2717240182291,47.8264553384537));
#16663=CARTESIAN_POINT('Ctrl Pts',(-57.3169558044938,25.2103549049237,47.7786797574698));
#16664=CARTESIAN_POINT('Ctrl Pts',(-57.5263914026889,25.0744920557659,47.7140189797529));
#16665=CARTESIAN_POINT('Ctrl Pts',(-57.6321855598595,24.9998579453427,47.6978257430375));
#16666=CARTESIAN_POINT('Ctrl Pts',(-57.7272582675279,24.92755355845,47.6978257430375));
#16667=CARTESIAN_POINT('',(-59.3886396402648,22.6860394732673,51.1464466094067));
#16668=CARTESIAN_POINT('Origin',(-54.7005384776276,20.9477335482704,52.8847525344037));
#16669=CARTESIAN_POINT('',(-59.2419176297992,23.0395928638606,52.));
#16670=CARTESIAN_POINT('Ctrl Pts',(-59.2419176297992,23.0395928638606,52.));
#16671=CARTESIAN_POINT('Ctrl Pts',(-59.2704596107889,22.9776288701721,52.));
#16672=CARTESIAN_POINT('Ctrl Pts',(-59.2996960329248,22.9104700099307,51.9877768144645));
#16673=CARTESIAN_POINT('Ctrl Pts',(-59.3511584515006,22.7852096676192,51.9357615493743));
#16674=CARTESIAN_POINT('Ctrl Pts',(-59.3734459899013,22.7271564800506,51.8959141016255));
#16675=CARTESIAN_POINT('Ctrl Pts',(-59.4060352501051,22.6389806710746,51.8052231982866));
#16676=CARTESIAN_POINT('Ctrl Pts',(-59.4191204951109,22.6017210834816,51.7501423324695));
#16677=CARTESIAN_POINT('Ctrl Pts',(-59.4362506414883,22.5520157275868,51.6287300770116));
#16678=CARTESIAN_POINT('Ctrl Pts',(-59.4403680019216,22.5395928638606,51.5623995455887));
#16679=CARTESIAN_POINT('Ctrl Pts',(-59.4403680019216,22.5395928638606,51.4376004544113));
#16680=CARTESIAN_POINT('Ctrl Pts',(-59.4362506414883,22.5520157275868,51.3712699229884));
#16681=CARTESIAN_POINT('Ctrl Pts',(-59.4191204951109,22.6017210834816,51.2498576675305));
#16682=CARTESIAN_POINT('Ctrl Pts',(-59.4060352501051,22.6389806710747,51.1947768017135));
#16683=CARTESIAN_POINT('Ctrl Pts',(-59.3898641102192,22.682734451694,51.1497750043391));
#16684=CARTESIAN_POINT('Ctrl Pts',(-59.389255015777,22.6843798444226,51.1481062382515));
#16685=CARTESIAN_POINT('Ctrl Pts',(-59.3886396402648,22.6860394732673,51.1464466094067));
#16686=CARTESIAN_POINT('',(-50.1591593254561,23.0395928638606,52.));
#16687=CARTESIAN_POINT('Origin',(-54.7005384776276,20.9477335482704,52.));
#16688=CARTESIAN_POINT('',(-50.0124373149904,22.6860394732673,51.1464466094067));
#16689=CARTESIAN_POINT('Ctrl Pts',(-50.0124373149904,22.6860394732673,51.1464466094067));
#16690=CARTESIAN_POINT('Ctrl Pts',(-50.0118219394782,22.6843798444226,51.1481062382515));
#16691=CARTESIAN_POINT('Ctrl Pts',(-50.011212845036,22.682734451694,51.1497750043391));
#16692=CARTESIAN_POINT('Ctrl Pts',(-49.9950417051501,22.6389806710746,51.1947768017134));
#16693=CARTESIAN_POINT('Ctrl Pts',(-49.9819564601444,22.6017210834816,51.2498576675305));
#16694=CARTESIAN_POINT('Ctrl Pts',(-49.964826313767,22.5520157275868,51.3712699229884));
#16695=CARTESIAN_POINT('Ctrl Pts',(-49.9607089533337,22.5395928638606,51.4376004544113));
#16696=CARTESIAN_POINT('Ctrl Pts',(-49.9607089533337,22.5395928638606,51.5623995455887));
#16697=CARTESIAN_POINT('Ctrl Pts',(-49.964826313767,22.5520157275868,51.6287300770116));
#16698=CARTESIAN_POINT('Ctrl Pts',(-49.9819564601444,22.6017210834816,51.7501423324695));
#16699=CARTESIAN_POINT('Ctrl Pts',(-49.9950417051502,22.6389806710747,51.8052231982866));
#16700=CARTESIAN_POINT('Ctrl Pts',(-50.0276309653539,22.7271564800506,51.8959141016255));
#16701=CARTESIAN_POINT('Ctrl Pts',(-50.0499185037546,22.7852096676192,51.9357615493743));
#16702=CARTESIAN_POINT('Ctrl Pts',(-50.1013809223305,22.9104700099307,51.9877768144645));
#16703=CARTESIAN_POINT('Ctrl Pts',(-50.1306173444663,22.9776288701721,52.));
#16704=CARTESIAN_POINT('Ctrl Pts',(-50.1591593254561,23.0395928638606,52.));
#16705=CARTESIAN_POINT('',(-52.2061698261501,25.2811069490433,48.5513791336308));
#16706=CARTESIAN_POINT('Origin',(-54.7005384776276,20.9477335482704,52.8847525344037));
#16707=CARTESIAN_POINT('',(-51.6738186877274,24.92755355845,47.6978257430375));
#16708=CARTESIAN_POINT('Ctrl Pts',(-51.6738186877274,24.92755355845,47.6978257430375));
#16709=CARTESIAN_POINT('Ctrl Pts',(-51.7688913953957,24.9998579453427,47.6978257430375));
#16710=CARTESIAN_POINT('Ctrl Pts',(-51.8746855525663,25.0744920557659,47.7140189797529));
#16711=CARTESIAN_POINT('Ctrl Pts',(-52.0841211507614,25.2103549049237,47.7786797574698));
#16712=CARTESIAN_POINT('Ctrl Pts',(-52.1878845511711,25.2717240182291,47.8264553384537));
#16713=CARTESIAN_POINT('Ctrl Pts',(-52.3259098194384,25.348221870878,47.9239881120561));
#16714=CARTESIAN_POINT('Ctrl Pts',(-52.3766609719605,25.3750874905218,47.9680392894922));
#16715=CARTESIAN_POINT('Ctrl Pts',(-52.434392279429,25.4047562084472,48.0459951427578));
#16716=CARTESIAN_POINT('Ctrl Pts',(-52.4505615795749,25.4129061770103,48.0739431957104));
#16717=CARTESIAN_POINT('Ctrl Pts',(-52.4733169725601,25.4242998143135,48.1333421546345));
#16718=CARTESIAN_POINT('Ctrl Pts',(-52.4799050823113,25.42755355845,48.1647903548472));
#16719=CARTESIAN_POINT('Ctrl Pts',(-52.4799050823113,25.42755355845,48.1978257430375));
#16720=CARTESIAN_POINT('Ctrl Pts',(-52.4799050823113,25.42755355845,48.2308611312278));
#16721=CARTESIAN_POINT('Ctrl Pts',(-52.4733169725601,25.4242998143135,48.2623093314405));
#16722=CARTESIAN_POINT('Ctrl Pts',(-52.4505615795749,25.4129061770103,48.3217082903646));
#16723=CARTESIAN_POINT('Ctrl Pts',(-52.434392279429,25.4047562084472,48.3496563433172));
#16724=CARTESIAN_POINT('Ctrl Pts',(-52.3766609719605,25.3750874905218,48.4276121965828));
#16725=CARTESIAN_POINT('Ctrl Pts',(-52.3259098194384,25.348221870878,48.4716633740189));
#16726=CARTESIAN_POINT('Ctrl Pts',(-52.2541268468932,25.3084375377237,48.522387364616));
#16727=CARTESIAN_POINT('Ctrl Pts',(-52.2305123905759,25.2951189724682,48.5373671102059));
#16728=CARTESIAN_POINT('Ctrl Pts',(-52.2061698261501,25.2811069490433,48.5513791336308));
#16729=CARTESIAN_POINT('Origin',(-54.7005384776276,20.9477335482704,47.6978257430375));
#16730=CARTESIAN_POINT('Origin',(8.29946152237238,41.9477335482704,64.));
#16731=CARTESIAN_POINT('',(13.2994615223724,41.9477335482704,64.));
#16732=CARTESIAN_POINT('Origin',(8.29946152237238,41.9477335482704,64.));
#16733=CARTESIAN_POINT('',(13.2994615223724,41.9477335482704,52.));
#16734=CARTESIAN_POINT('',(13.2994615223724,41.9477335482704,64.));
#16735=CARTESIAN_POINT('Origin',(8.29946152237238,41.9477335482704,52.));
#16736=CARTESIAN_POINT('Origin',(-33.7005384776276,-41.9477335482704,64.));
#16737=CARTESIAN_POINT('',(-28.7005384776276,-41.9477335482704,64.));
#16738=CARTESIAN_POINT('Origin',(-33.7005384776276,-41.9477335482704,64.));
#16739=CARTESIAN_POINT('',(-28.7005384776276,-41.9477335482704,64.));
#16740=CARTESIAN_POINT('',(-29.612959590116,-44.8272645584125,48.1978257430375));
#16741=CARTESIAN_POINT('Ctrl Pts',(-29.612959590116,-44.8272645584125,48.1978257430375));
#16742=CARTESIAN_POINT('Ctrl Pts',(-29.612959590116,-44.8272645584125,48.1321584122493));
#16743=CARTESIAN_POINT('Ctrl Pts',(-29.6032015594757,-44.8135380049881,
48.0636994127672));
#16744=CARTESIAN_POINT('Ctrl Pts',(-29.5671921138605,-44.7613527165994,
47.9408836439009));
#16745=CARTESIAN_POINT('Ctrl Pts',(-29.5411446978572,-44.7229773515989,
47.8864317550374));
#16746=CARTESIAN_POINT('Ctrl Pts',(-29.483890379582,-44.6352673224994,47.7987217259379));
#16747=CARTESIAN_POINT('Ctrl Pts',(-29.4481192034526,-44.5787128115292,
47.7605853033887));
#16748=CARTESIAN_POINT('Ctrl Pts',(-29.3745620549058,-44.4559300231491,
47.710126421675));
#16749=CARTESIAN_POINT('Ctrl Pts',(-29.3368235722438,-44.3896643528756,
47.6978257430375));
#16750=CARTESIAN_POINT('Ctrl Pts',(-29.3030582705349,-44.3272645584124,
47.6978257430375));
#16751=CARTESIAN_POINT('',(-29.612959590116,-44.8272645584124,51.5));
#16752=CARTESIAN_POINT('',(-29.612959590116,-44.8272645584125,64.));
#16753=CARTESIAN_POINT('',(-30.0156001943604,-45.3272645584124,52.));
#16754=CARTESIAN_POINT('Ctrl Pts',(-30.0156001943604,-45.3272645584124,
52.));
#16755=CARTESIAN_POINT('Ctrl Pts',(-29.9626248485631,-45.269501845417,52.));
#16756=CARTESIAN_POINT('Ctrl Pts',(-29.90662334431,-45.2054409446566,51.9894566895945));
#16757=CARTESIAN_POINT('Ctrl Pts',(-29.8039582965593,-45.0819180329636,
51.9406971089121));
#16758=CARTESIAN_POINT('Ctrl Pts',(-29.7572642176841,-45.0225259231798,
51.9023681459539));
#16759=CARTESIAN_POINT('Ctrl Pts',(-29.6887928314324,-44.9324583590974,
51.8123005818715));
#16760=CARTESIAN_POINT('Ctrl Pts',(-29.6606197247029,-44.8939359317371,
51.7582688558033));
#16761=CARTESIAN_POINT('Ctrl Pts',(-29.622738109016,-44.8412774147571,51.6352518100092));
#16762=CARTESIAN_POINT('Ctrl Pts',(-29.612959590116,-44.8272645584124,51.5662353407203));
#16763=CARTESIAN_POINT('Ctrl Pts',(-29.612959590116,-44.8272645584124,51.5));
#16764=CARTESIAN_POINT('',(-37.3854767608948,-45.3272645584124,52.));
#16765=CARTESIAN_POINT('Origin',(-33.7005384776276,-41.9477335482704,52.));
#16766=CARTESIAN_POINT('',(-37.7881173651392,-44.8272645584124,51.5));
#16767=CARTESIAN_POINT('Ctrl Pts',(-37.7881173651392,-44.8272645584124,
51.5));
#16768=CARTESIAN_POINT('Ctrl Pts',(-37.7881173651392,-44.8272645584124,
51.5662353407203));
#16769=CARTESIAN_POINT('Ctrl Pts',(-37.7783388462392,-44.8412774147571,
51.6352518100092));
#16770=CARTESIAN_POINT('Ctrl Pts',(-37.7404572305523,-44.8939359317371,
51.7582688558033));
#16771=CARTESIAN_POINT('Ctrl Pts',(-37.7122841238229,-44.9324583590974,
51.8123005818715));
#16772=CARTESIAN_POINT('Ctrl Pts',(-37.6438127375711,-45.0225259231798,
51.9023681459539));
#16773=CARTESIAN_POINT('Ctrl Pts',(-37.5971186586959,-45.0819180329636,
51.9406971089121));
#16774=CARTESIAN_POINT('Ctrl Pts',(-37.4944536109452,-45.2054409446566,
51.9894566895945));
#16775=CARTESIAN_POINT('Ctrl Pts',(-37.4384521066922,-45.269501845417,52.));
#16776=CARTESIAN_POINT('Ctrl Pts',(-37.3854767608948,-45.3272645584124,
52.));
#16777=CARTESIAN_POINT('',(-37.7881173651392,-44.8272645584125,48.1978257430375));
#16778=CARTESIAN_POINT('',(-37.7881173651392,-44.8272645584125,64.));
#16779=CARTESIAN_POINT('Ctrl Pts',(-38.0980186847204,-44.3272645584124,
47.6978257430375));
#16780=CARTESIAN_POINT('Ctrl Pts',(-38.0642533830114,-44.3896643528756,
47.6978257430375));
#16781=CARTESIAN_POINT('Ctrl Pts',(-38.0265149003494,-44.4559300231491,
47.710126421675));
#16782=CARTESIAN_POINT('Ctrl Pts',(-37.9529577518027,-44.5787128115292,
47.7605853033887));
#16783=CARTESIAN_POINT('Ctrl Pts',(-37.9171865756733,-44.6352673224994,
47.7987217259379));
#16784=CARTESIAN_POINT('Ctrl Pts',(-37.859932257398,-44.7229773515989,47.8864317550374));
#16785=CARTESIAN_POINT('Ctrl Pts',(-37.8338848413947,-44.7613527165994,
47.9408836439009));
#16786=CARTESIAN_POINT('Ctrl Pts',(-37.7978753957795,-44.8135380049881,
48.0636994127672));
#16787=CARTESIAN_POINT('Ctrl Pts',(-37.7881173651392,-44.8272645584124,
48.1321584122493));
#16788=CARTESIAN_POINT('Ctrl Pts',(-37.7881173651392,-44.8272645584124,
48.1978257430375));
#16789=CARTESIAN_POINT('Origin',(-90.,-22.0741207385023,47.1978257430375));
#16790=CARTESIAN_POINT('',(-90.,-21.5741207385023,47.1978257430375));
#16791=CARTESIAN_POINT('Origin',(-90.,-22.0741207385023,47.1978257430375));
#16792=CARTESIAN_POINT('',(-89.5,-21.5741207385023,47.1978257430375));
#16793=CARTESIAN_POINT('Origin',(-89.5,-22.0741207385023,47.1978257430375));
#16794=CARTESIAN_POINT('',(-90.,-21.5741207385023,47.1978257430375));
#16795=CARTESIAN_POINT('Origin',(-90.,-22.0741207385023,47.1978257430375));
#16796=CARTESIAN_POINT('',(-90.,-21.5741207385023,47.1978257430375));
#16797=CARTESIAN_POINT('Origin',(-90.,-22.0741207385023,47.1978257430375));
#16798=CARTESIAN_POINT('',(89.5,-21.5741207385024,47.1978257430375));
#16799=CARTESIAN_POINT('',(-90.,-21.5741207385023,47.1978257430375));
#16800=CARTESIAN_POINT('Origin',(89.5,-22.0741207385024,47.1978257430375));
#16801=CARTESIAN_POINT('Origin',(-90.,-22.0741207385023,47.1978257430375));
#16802=CARTESIAN_POINT('',(-90.,-21.5741207385023,47.1978257430375));
#16803=CARTESIAN_POINT('Origin',(-90.,-21.5741207385023,35.6978257430375));
#16804=CARTESIAN_POINT('',(89.5,-21.5741207385024,36.1978257430375));
#16805=CARTESIAN_POINT('',(-90.,-21.5741207385023,36.1978257430375));
#16806=CARTESIAN_POINT('',(89.5,-21.5741207385024,43.8489128715187));
#16807=CARTESIAN_POINT('Origin',(-90.,-21.5741207385023,35.6978257430375));
#16808=CARTESIAN_POINT('',(-90.,-21.5741207385023,36.1978257430375));
#16809=CARTESIAN_POINT('Origin',(-90.,-21.5741207385023,35.6978257430375));
#16810=CARTESIAN_POINT('',(-89.5,-21.5741207385023,36.1978257430375));
#16811=CARTESIAN_POINT('',(-89.5,-21.5741207385023,43.8489128715187));
#16812=CARTESIAN_POINT('',(-90.,-21.5741207385023,36.1978257430375));
#16813=CARTESIAN_POINT('Origin',(-90.,-21.5741207385023,35.6978257430375));
#16814=CARTESIAN_POINT('',(-90.,-21.5741207385023,36.1978257430375));
#16815=CARTESIAN_POINT('Origin',(-90.,-21.0741207385023,36.1978257430375));
#16816=CARTESIAN_POINT('',(-90.,-21.0741207385023,35.6978257430375));
#16817=CARTESIAN_POINT('Origin',(-90.,-21.0741207385023,36.1978257430375));
#16818=CARTESIAN_POINT('',(-89.5,-21.0741207385023,35.6978257430375));
#16819=CARTESIAN_POINT('Origin',(-89.5,-21.0741207385023,36.1978257430375));
#16820=CARTESIAN_POINT('',(-90.,-21.0741207385023,35.6978257430375));
#16821=CARTESIAN_POINT('Origin',(-90.,-21.0741207385023,36.1978257430375));
#16822=CARTESIAN_POINT('',(-90.,-21.0741207385023,35.6978257430375));
#16823=CARTESIAN_POINT('Origin',(-90.,-21.0741207385023,36.1978257430375));
#16824=CARTESIAN_POINT('',(89.5,-21.0741207385024,35.6978257430375));
#16825=CARTESIAN_POINT('',(-90.,-21.0741207385023,35.6978257430375));
#16826=CARTESIAN_POINT('Origin',(89.5,-21.0741207385024,36.1978257430375));
#16827=CARTESIAN_POINT('Origin',(-90.,18.5453000725091,36.1978257430375));
#16828=CARTESIAN_POINT('',(-89.5,18.5453000725091,35.6978257430375));
#16829=CARTESIAN_POINT('',(-90.,18.5453000725091,35.6978257430375));
#16830=CARTESIAN_POINT('',(-89.5,19.0453000725091,36.1978257430375));
#16831=CARTESIAN_POINT('Origin',(-89.5,18.5453000725091,36.1978257430375));
#16832=CARTESIAN_POINT('',(-90.,19.0453000725091,36.1978257430375));
#16833=CARTESIAN_POINT('Origin',(-90.,18.5453000725091,36.1978257430375));
#16834=CARTESIAN_POINT('',(-90.,18.5453000725091,35.6978257430375));
#16835=CARTESIAN_POINT('',(-90.,19.0453000725091,36.1978257430375));
#16836=CARTESIAN_POINT('Origin',(-90.,18.5453000725091,36.1978257430375));
#16837=CARTESIAN_POINT('',(89.5,19.045300072509,36.1978257430375));
#16838=CARTESIAN_POINT('',(-90.,19.0453000725091,36.1978257430375));
#16839=CARTESIAN_POINT('',(89.5,18.545300072509,35.6978257430375));
#16840=CARTESIAN_POINT('Origin',(89.5,18.545300072509,36.1978257430375));
#16841=CARTESIAN_POINT('',(-90.,18.5453000725091,35.6978257430375));
#16842=CARTESIAN_POINT('Origin',(-90.,18.5453000725091,36.1978257430375));
#16843=CARTESIAN_POINT('',(-90.,19.0453000725091,36.1978257430375));
#16844=CARTESIAN_POINT('',(-90.,18.5453000725091,35.6978257430375));
#16845=CARTESIAN_POINT('Origin',(-90.,18.5453000725091,36.1978257430375));
#16846=CARTESIAN_POINT('',(-90.,18.5453000725091,35.6978257430375));
#16847=CARTESIAN_POINT('',(-90.,19.0453000725091,36.1978257430375));
#16848=CARTESIAN_POINT('Origin',(-90.,19.0453000725091,47.6978257430375));
#16849=CARTESIAN_POINT('',(-89.5,19.0453000725091,47.1978257430375));
#16850=CARTESIAN_POINT('',(-89.5,19.0453000725091,49.8489128715187));
#16851=CARTESIAN_POINT('',(-90.,19.0453000725091,47.1978257430375));
#16852=CARTESIAN_POINT('Origin',(-90.,19.0453000725091,47.6978257430375));
#16853=CARTESIAN_POINT('',(-90.,19.0453000725091,47.1978257430375));
#16854=CARTESIAN_POINT('Origin',(-90.,19.0453000725091,47.6978257430375));
#16855=CARTESIAN_POINT('',(89.5,19.045300072509,47.1978257430375));
#16856=CARTESIAN_POINT('',(-90.,19.0453000725091,47.1978257430375));
#16857=CARTESIAN_POINT('',(89.5,19.045300072509,49.8489128715187));
#16858=CARTESIAN_POINT('Origin',(-90.,19.0453000725091,47.6978257430375));
#16859=CARTESIAN_POINT('',(-90.,19.0453000725091,47.1978257430375));
#16860=CARTESIAN_POINT('Origin',(-90.,19.0453000725091,47.6978257430375));
#16861=CARTESIAN_POINT('',(-90.,19.0453000725091,47.1978257430375));
#16862=CARTESIAN_POINT('Origin',(-45.,23.0395928638606,51.5));
#16863=CARTESIAN_POINT('',(-89.5,22.6860394732674,51.1464466094067));
#16864=CARTESIAN_POINT('',(-45.,22.6860394732673,51.1464466094067));
#16865=CARTESIAN_POINT('',(-89.5,23.0395928638606,52.));
#16866=CARTESIAN_POINT('Origin',(-89.5,23.0395928638606,51.5));
#16867=CARTESIAN_POINT('',(-45.,23.0395928638606,52.));
#16868=CARTESIAN_POINT('Origin',(-45.,23.0395928638606,51.5));
#16869=CARTESIAN_POINT('',(-45.,22.6860394732673,51.1464466094067));
#16870=CARTESIAN_POINT('',(-45.,23.0395928638606,52.));
#16871=CARTESIAN_POINT('Origin',(-45.,23.0395928638606,51.5));
#16872=CARTESIAN_POINT('',(89.5,23.0395928638606,52.));
#16873=CARTESIAN_POINT('',(-45.,23.0395928638606,52.));
#16874=CARTESIAN_POINT('',(89.5,22.6860394732673,51.1464466094067));
#16875=CARTESIAN_POINT('Origin',(89.5,23.0395928638606,51.5));
#16876=CARTESIAN_POINT('',(-45.,22.6860394732673,51.1464466094067));
#16877=CARTESIAN_POINT('Origin',(-45.,23.0395928638606,51.5));
#16878=CARTESIAN_POINT('',(-45.,23.0395928638606,52.));
#16879=CARTESIAN_POINT('',(-45.,22.6860394732673,51.1464466094067));
#16880=CARTESIAN_POINT('Origin',(-90.,19.5453000725091,47.1978257430375));
#16881=CARTESIAN_POINT('',(-89.5,19.5453000725091,47.6978257430375));
#16882=CARTESIAN_POINT('Origin',(-89.5,19.5453000725091,47.1978257430375));
#16883=CARTESIAN_POINT('',(-90.,19.5453000725091,47.6978257430375));
#16884=CARTESIAN_POINT('Origin',(-90.,19.5453000725091,47.1978257430375));
#16885=CARTESIAN_POINT('',(-90.,19.5453000725091,47.6978257430375));
#16886=CARTESIAN_POINT('Origin',(-90.,19.5453000725091,47.1978257430375));
#16887=CARTESIAN_POINT('',(89.5,19.545300072509,47.6978257430375));
#16888=CARTESIAN_POINT('',(-90.,19.5453000725091,47.6978257430375));
#16889=CARTESIAN_POINT('Origin',(89.5,19.545300072509,47.1978257430375));
#16890=CARTESIAN_POINT('Origin',(-90.,19.5453000725091,47.1978257430375));
#16891=CARTESIAN_POINT('',(-90.,19.5453000725091,47.6978257430375));
#16892=CARTESIAN_POINT('Origin',(-90.,19.5453000725091,47.1978257430375));
#16893=CARTESIAN_POINT('',(-90.,19.5453000725091,47.6978257430375));
#16894=CARTESIAN_POINT('Origin',(-90.,21.8324860826741,52.));
#16895=CARTESIAN_POINT('',(-89.5,25.2811069490433,48.5513791336308));
#16896=CARTESIAN_POINT('',(-90.,25.2811069490433,48.5513791336308));
#16897=CARTESIAN_POINT('',(-89.5,32.6243645620056,41.2081215206685));
#16898=CARTESIAN_POINT('Origin',(-90.,21.8324860826741,52.));
#16899=CARTESIAN_POINT('',(-90.,25.2811069490433,48.5513791336308));
#16900=CARTESIAN_POINT('Origin',(-90.,21.8324860826741,52.));
#16901=CARTESIAN_POINT('',(89.5,25.2811069490433,48.5513791336308));
#16902=CARTESIAN_POINT('',(89.5,0.124364562005535,73.7081215206685));
#16903=CARTESIAN_POINT('',(-90.,25.2811069490433,48.5513791336308));
#16904=CARTESIAN_POINT('Origin',(-90.,21.8324860826741,52.));
#16905=CARTESIAN_POINT('',(-90.,25.2811069490433,48.5513791336308));
#16906=CARTESIAN_POINT('Origin',(-90.,26.1346603396366,47.6978257430375));
#16907=CARTESIAN_POINT('',(89.5,24.92755355845,47.6978257430375));
#16908=CARTESIAN_POINT('',(-90.,24.92755355845,47.6978257430375));
#16909=CARTESIAN_POINT('',(89.5,-19.4326698301817,47.6978257430375));
#16910=CARTESIAN_POINT('Origin',(-90.,26.1346603396366,47.6978257430375));
#16911=CARTESIAN_POINT('',(-89.5,24.92755355845,47.6978257430375));
#16912=CARTESIAN_POINT('',(-89.5,45.5673301698183,47.6978257430375));
#16913=CARTESIAN_POINT('',(-90.,24.92755355845,47.6978257430375));
#16914=CARTESIAN_POINT('Origin',(-90.,26.1346603396366,47.6978257430375));
#16915=CARTESIAN_POINT('',(-90.,24.92755355845,47.6978257430375));
#16916=CARTESIAN_POINT('Origin',(-90.,26.1346603396366,47.6978257430375));
#16917=CARTESIAN_POINT('',(-90.,24.92755355845,47.6978257430375));
#16918=CARTESIAN_POINT('Origin',(-90.,24.92755355845,48.1978257430375));
#16919=CARTESIAN_POINT('Origin',(-89.5,24.92755355845,48.1978257430375));
#16920=CARTESIAN_POINT('Origin',(-90.,24.92755355845,48.1978257430375));
#16921=CARTESIAN_POINT('Origin',(-90.,24.92755355845,48.1978257430375));
#16922=CARTESIAN_POINT('Origin',(89.5,24.92755355845,48.1978257430375));
#16923=CARTESIAN_POINT('Origin',(-90.,24.92755355845,48.1978257430375));
#16924=CARTESIAN_POINT('Origin',(0.,0.,52.));
#16925=CARTESIAN_POINT('',(-45.,-45.3272645584124,52.));
#16926=CARTESIAN_POINT('',(-45.,-45.3272645584124,52.));
#16927=CARTESIAN_POINT('',(-45.,-45.3272645584124,52.));
#16928=CARTESIAN_POINT('',(-45.,-45.3272645584124,52.));
#16929=CARTESIAN_POINT('',(89.5,-45.3272645584125,52.));
#16930=CARTESIAN_POINT('',(-45.,-45.3272645584124,52.));
#16931=CARTESIAN_POINT('',(89.5,-64.5,52.));
#16932=CARTESIAN_POINT('',(89.5,-32.5,52.));
#16933=CARTESIAN_POINT('',(-89.5,-64.5,52.));
#16934=CARTESIAN_POINT('',(-45.,-64.5,52.));
#16935=CARTESIAN_POINT('',(-89.5,32.5,52.));
#16936=CARTESIAN_POINT('Origin',(-45.,-45.3272645584124,51.5));
#16937=CARTESIAN_POINT('',(-45.,-44.8272645584124,51.5));
#16938=CARTESIAN_POINT('Origin',(-45.,-45.3272645584124,51.5));
#16939=CARTESIAN_POINT('',(89.5,-44.8272645584125,51.5));
#16940=CARTESIAN_POINT('',(-45.,-44.8272645584124,51.5));
#16941=CARTESIAN_POINT('Origin',(89.5,-45.3272645584125,51.5));
#16942=CARTESIAN_POINT('Origin',(-45.,-45.3272645584124,51.5));
#16943=CARTESIAN_POINT('',(-45.,-44.8272645584124,51.5));
#16944=CARTESIAN_POINT('Origin',(-45.,-45.3272645584124,51.5));
#16945=CARTESIAN_POINT('',(-45.,-44.8272645584124,51.5));
#16946=CARTESIAN_POINT('Origin',(-45.,-45.3272645584124,51.5));
#16947=CARTESIAN_POINT('',(-45.,-44.8272645584124,51.5));
#16948=CARTESIAN_POINT('Origin',(-90.,-44.8272645584124,47.6978257430375));
#16949=CARTESIAN_POINT('',(89.5,-44.8272645584125,48.1978257430375));
#16950=CARTESIAN_POINT('',(-90.,-44.8272645584124,48.1978257430375));
#16951=CARTESIAN_POINT('',(89.5,-44.8272645584125,49.8489128715187));
#16952=CARTESIAN_POINT('Origin',(-90.,-44.8272645584124,47.6978257430375));
#16953=CARTESIAN_POINT('',(-90.,-44.8272645584124,48.1978257430375));
#16954=CARTESIAN_POINT('Origin',(-90.,-44.8272645584124,47.6978257430375));
#16955=CARTESIAN_POINT('',(-90.,-44.8272645584124,48.1978257430375));
#16956=CARTESIAN_POINT('Origin',(-90.,-44.8272645584124,47.6978257430375));
#16957=CARTESIAN_POINT('',(-90.,-44.8272645584124,48.1978257430375));
#16958=CARTESIAN_POINT('Origin',(-90.,-44.3272645584124,48.1978257430375));
#16959=CARTESIAN_POINT('Origin',(-90.,-44.3272645584124,48.1978257430375));
#16960=CARTESIAN_POINT('Origin',(89.5,-44.3272645584125,48.1978257430375));
#16961=CARTESIAN_POINT('Origin',(-90.,-44.3272645584124,48.1978257430375));
#16962=CARTESIAN_POINT('Origin',(-90.,-44.3272645584124,48.1978257430375));
#16963=CARTESIAN_POINT('Origin',(-90.,19.0453000725091,35.6978257430375));
#16964=CARTESIAN_POINT('',(-90.,-21.0741207385023,35.6978257430375));
#16965=CARTESIAN_POINT('',(-89.5,42.0226500362545,35.6978257430375));
#16966=CARTESIAN_POINT('',(89.5,-22.9773499637455,35.6978257430375));
#16967=CARTESIAN_POINT('Origin',(0.,0.,52.));
#16968=CARTESIAN_POINT('',(-45.,23.0395928638606,52.));
#16969=CARTESIAN_POINT('',(-89.5,64.5,52.));
#16970=CARTESIAN_POINT('',(-89.5,32.5,52.));
#16971=CARTESIAN_POINT('',(89.5,64.5,52.));
#16972=CARTESIAN_POINT('',(45.,64.5,52.));
#16973=CARTESIAN_POINT('',(89.5,-32.5,52.));
#16974=CARTESIAN_POINT('Origin',(89.5,24.92755355845,48.1978257430375));
#16975=CARTESIAN_POINT('',(90.,24.92755355845,48.1978257430375));
#16976=CARTESIAN_POINT('Origin',(89.5,24.92755355845,48.1978257430375));
#16977=CARTESIAN_POINT('Origin',(89.5,24.92755355845,48.1978257430375));
#16978=CARTESIAN_POINT('Origin',(-89.5,24.92755355845,48.1978257430375));
#16979=CARTESIAN_POINT('',(-90.,24.92755355845,48.1978257430375));
#16980=CARTESIAN_POINT('Origin',(-89.5,24.92755355845,48.1978257430375));
#16981=CARTESIAN_POINT('Origin',(-89.5,24.92755355845,48.1978257430375));
#16982=CARTESIAN_POINT('Origin',(89.5,19.545300072509,47.1978257430375));
#16983=CARTESIAN_POINT('',(90.,19.545300072509,48.1978257430375));
#16984=CARTESIAN_POINT('Origin',(89.5,19.545300072509,48.1978257430375));
#16985=CARTESIAN_POINT('',(90.,18.545300072509,47.1978257430375));
#16986=CARTESIAN_POINT('Origin',(90.,19.545300072509,47.1978257430375));
#16987=CARTESIAN_POINT('Origin',(89.5,18.545300072509,47.1978257430375));
#16988=CARTESIAN_POINT('Origin',(89.5,-19.4326698301817,48.1978257430375));
#16989=CARTESIAN_POINT('',(90.,-19.4326698301817,48.1978257430375));
#16990=CARTESIAN_POINT('Origin',(89.5,23.0395928638606,51.5));
#16991=CARTESIAN_POINT('',(90.,23.0395928638606,52.5));
#16992=CARTESIAN_POINT('',(90.,22.3324860826741,50.7928932188135));
#16993=CARTESIAN_POINT('Origin',(90.,23.0395928638606,51.5));
#16994=CARTESIAN_POINT('Origin',(89.5,22.332486082674,50.7928932188135));
#16995=CARTESIAN_POINT('Origin',(89.5,23.0395928638606,52.5));
#16996=CARTESIAN_POINT('Origin',(-89.5,19.5453000725091,47.1978257430375));
#16997=CARTESIAN_POINT('',(-90.,18.5453000725091,47.1978257430375));
#16998=CARTESIAN_POINT('Origin',(-89.5,18.5453000725091,47.1978257430375));
#16999=CARTESIAN_POINT('',(-90.,19.5453000725091,48.1978257430375));
#17000=CARTESIAN_POINT('Origin',(-90.,19.5453000725091,47.1978257430375));
#17001=CARTESIAN_POINT('Origin',(-89.5,19.5453000725091,48.1978257430375));
#17002=CARTESIAN_POINT('Origin',(-89.5,23.0395928638606,51.5));
#17003=CARTESIAN_POINT('',(-90.,22.3324860826741,50.7928932188135));
#17004=CARTESIAN_POINT('',(-90.,23.0395928638606,52.5));
#17005=CARTESIAN_POINT('Origin',(-90.,23.0395928638606,51.5));
#17006=CARTESIAN_POINT('Origin',(-89.5,23.0395928638606,52.5));
#17007=CARTESIAN_POINT('Origin',(-89.5,22.3324860826741,50.7928932188135));
#17008=CARTESIAN_POINT('Origin',(-89.5,32.2708111714123,40.8545681300752));
#17009=CARTESIAN_POINT('',(-90.,32.2708111714123,40.8545681300752));
#17010=CARTESIAN_POINT('Origin',(89.5,18.545300072509,36.1978257430375));
#17011=CARTESIAN_POINT('',(90.,18.545300072509,36.1978257430375));
#17012=CARTESIAN_POINT('Origin',(89.5,18.545300072509,36.1978257430375));
#17013=CARTESIAN_POINT('Origin',(89.5,18.545300072509,36.1978257430375));
#17014=CARTESIAN_POINT('Origin',(89.5,18.545300072509,49.8489128715187));
#17015=CARTESIAN_POINT('',(90.,18.545300072509,49.8489128715187));
#17016=CARTESIAN_POINT('Origin',(89.5,64.5,52.5));
#17017=CARTESIAN_POINT('',(90.,64.5,52.5));
#17018=CARTESIAN_POINT('',(89.5,65.,52.5));
#17019=CARTESIAN_POINT('Origin',(89.5,64.5,52.5));
#17020=CARTESIAN_POINT('Origin',(89.5,64.5,52.5));
#17021=CARTESIAN_POINT('Origin',(89.5,64.5,52.5));
#17022=CARTESIAN_POINT('Origin',(89.5,-32.5,52.5));
#17023=CARTESIAN_POINT('',(90.,-32.5,52.5));
#17024=CARTESIAN_POINT('Origin',(-89.5,18.5453000725091,36.1978257430375));
#17025=CARTESIAN_POINT('',(-90.,18.5453000725091,36.1978257430375));
#17026=CARTESIAN_POINT('Origin',(-89.5,18.5453000725091,36.1978257430375));
#17027=CARTESIAN_POINT('Origin',(-89.5,18.5453000725091,36.1978257430375));
#17028=CARTESIAN_POINT('Origin',(-89.5,64.5,52.5));
#17029=CARTESIAN_POINT('',(-89.5,65.,52.5));
#17030=CARTESIAN_POINT('Origin',(-89.5,64.5,52.5));
#17031=CARTESIAN_POINT('',(-90.,64.5,52.5));
#17032=CARTESIAN_POINT('Origin',(-89.5,64.5,52.5));
#17033=CARTESIAN_POINT('Origin',(-89.5,64.5,52.5));
#17034=CARTESIAN_POINT('Origin',(-89.5,32.5,52.5));
#17035=CARTESIAN_POINT('',(-90.,32.5,52.5));
#17036=CARTESIAN_POINT('Origin',(89.5,-21.0741207385024,36.1978257430375));
#17037=CARTESIAN_POINT('',(90.,-21.0741207385024,36.1978257430375));
#17038=CARTESIAN_POINT('Origin',(89.5,-21.0741207385024,36.1978257430375));
#17039=CARTESIAN_POINT('Origin',(89.5,-21.0741207385024,36.1978257430375));
#17040=CARTESIAN_POINT('Origin',(89.5,-22.9773499637455,36.1978257430375));
#17041=CARTESIAN_POINT('',(90.,-22.9773499637455,36.1978257430375));
#17042=CARTESIAN_POINT('Origin',(89.5,64.5,63.5));
#17043=CARTESIAN_POINT('',(90.,64.5,63.5));
#17044=CARTESIAN_POINT('',(89.5,64.5,64.));
#17045=CARTESIAN_POINT('Origin',(89.5,64.5,63.5));
#17046=CARTESIAN_POINT('',(89.5,65.,63.5));
#17047=CARTESIAN_POINT('Origin',(89.5,64.5,63.5));
#17048=CARTESIAN_POINT('Origin',(89.5,64.5,63.5));
#17049=CARTESIAN_POINT('Origin',(89.5,64.5,52.));
#17050=CARTESIAN_POINT('',(90.,64.5,52.));
#17051=CARTESIAN_POINT('',(89.5,65.,52.));
#17052=CARTESIAN_POINT('Origin',(-89.5,-21.0741207385023,36.1978257430375));
#17053=CARTESIAN_POINT('',(-90.,-21.0741207385023,36.1978257430375));
#17054=CARTESIAN_POINT('Origin',(-89.5,-21.0741207385023,36.1978257430375));
#17055=CARTESIAN_POINT('Origin',(-89.5,-21.0741207385023,36.1978257430375));
#17056=CARTESIAN_POINT('Origin',(-89.5,64.5,63.5));
#17057=CARTESIAN_POINT('',(-89.5,65.,63.5));
#17058=CARTESIAN_POINT('',(-89.5,64.5,64.));
#17059=CARTESIAN_POINT('Origin',(-89.5,64.5,63.5));
#17060=CARTESIAN_POINT('',(-90.,64.5,63.5));
#17061=CARTESIAN_POINT('Origin',(-89.5,64.5,63.5));
#17062=CARTESIAN_POINT('Origin',(-89.5,64.5,63.5));
#17063=CARTESIAN_POINT('Origin',(-89.5,64.5,52.));
#17064=CARTESIAN_POINT('',(-89.5,65.,52.));
#17065=CARTESIAN_POINT('',(-90.,64.5,52.));
#17066=CARTESIAN_POINT('Origin',(89.5,-22.0741207385024,47.1978257430375));
#17067=CARTESIAN_POINT('',(90.,-21.0741207385024,47.1978257430375));
#17068=CARTESIAN_POINT('Origin',(89.5,-21.0741207385024,47.1978257430375));
#17069=CARTESIAN_POINT('',(90.,-22.0741207385024,48.1978257430375));
#17070=CARTESIAN_POINT('Origin',(90.,-22.0741207385024,47.1978257430375));
#17071=CARTESIAN_POINT('Origin',(89.5,-22.0741207385024,48.1978257430375));
#17072=CARTESIAN_POINT('Origin',(89.5,-21.0741207385024,43.8489128715187));
#17073=CARTESIAN_POINT('',(90.,-21.0741207385024,43.8489128715187));
#17074=CARTESIAN_POINT('Origin',(89.5,-64.5,63.5));
#17075=CARTESIAN_POINT('',(89.5,-65.,63.5));
#17076=CARTESIAN_POINT('',(89.5,-64.5,64.));
#17077=CARTESIAN_POINT('Origin',(89.5,-64.5,63.5));
#17078=CARTESIAN_POINT('',(90.,-64.5,63.5));
#17079=CARTESIAN_POINT('Origin',(89.5,-64.5,63.5));
#17080=CARTESIAN_POINT('Origin',(89.5,-64.5,63.5));
#17081=CARTESIAN_POINT('Origin',(-89.5,-22.0741207385023,47.1978257430375));
#17082=CARTESIAN_POINT('',(-90.,-22.0741207385023,48.1978257430375));
#17083=CARTESIAN_POINT('Origin',(-89.5,-22.0741207385023,48.1978257430375));
#17084=CARTESIAN_POINT('',(-90.,-21.0741207385023,47.1978257430375));
#17085=CARTESIAN_POINT('Origin',(-90.,-22.0741207385023,47.1978257430375));
#17086=CARTESIAN_POINT('Origin',(-89.5,-21.0741207385023,47.1978257430375));
#17087=CARTESIAN_POINT('Origin',(-89.5,-64.5,63.5));
#17088=CARTESIAN_POINT('',(-90.,-64.5,63.5));
#17089=CARTESIAN_POINT('',(-89.5,-64.5,64.));
#17090=CARTESIAN_POINT('Origin',(-89.5,-64.5,63.5));
#17091=CARTESIAN_POINT('',(-89.5,-65.,63.5));
#17092=CARTESIAN_POINT('Origin',(-89.5,-64.5,63.5));
#17093=CARTESIAN_POINT('Origin',(-89.5,-64.5,63.5));
#17094=CARTESIAN_POINT('Origin',(89.5,-44.3272645584125,48.1978257430375));
#17095=CARTESIAN_POINT('',(90.,-44.3272645584125,48.1978257430375));
#17096=CARTESIAN_POINT('Origin',(89.5,-44.3272645584125,48.1978257430375));
#17097=CARTESIAN_POINT('Origin',(89.5,-44.3272645584125,48.1978257430375));
#17098=CARTESIAN_POINT('Origin',(89.5,-43.2870603692512,48.1978257430375));
#17099=CARTESIAN_POINT('',(90.,-43.2870603692512,48.1978257430375));
#17100=CARTESIAN_POINT('Origin',(89.5,-64.5,52.5));
#17101=CARTESIAN_POINT('',(89.5,-65.,52.5));
#17102=CARTESIAN_POINT('',(90.,-64.5,52.5));
#17103=CARTESIAN_POINT('Origin',(89.5,-64.5,52.5));
#17104=CARTESIAN_POINT('Origin',(89.5,-64.5,52.5));
#17105=CARTESIAN_POINT('Origin',(89.5,-64.5,52.5));
#17106=CARTESIAN_POINT('Origin',(-89.5,-44.3272645584124,48.1978257430375));
#17107=CARTESIAN_POINT('',(-90.,-44.3272645584124,48.1978257430375));
#17108=CARTESIAN_POINT('Origin',(-89.5,-44.3272645584124,48.1978257430375));
#17109=CARTESIAN_POINT('Origin',(-89.5,-44.3272645584124,48.1978257430375));
#17110=CARTESIAN_POINT('Origin',(-89.5,-64.5,52.5));
#17111=CARTESIAN_POINT('',(-90.,-64.5,52.5));
#17112=CARTESIAN_POINT('',(-89.5,-65.,52.5));
#17113=CARTESIAN_POINT('Origin',(-89.5,-64.5,52.5));
#17114=CARTESIAN_POINT('Origin',(-89.5,-64.5,52.5));
#17115=CARTESIAN_POINT('Origin',(-89.5,-64.5,52.5));
#17116=CARTESIAN_POINT('Origin',(89.5,-45.3272645584125,51.5));
#17117=CARTESIAN_POINT('',(90.,-44.3272645584125,51.5));
#17118=CARTESIAN_POINT('Origin',(89.5,-44.3272645584125,51.5));
#17119=CARTESIAN_POINT('',(90.,-45.3272645584125,52.5));
#17120=CARTESIAN_POINT('Origin',(90.,-45.3272645584125,51.5));
#17121=CARTESIAN_POINT('Origin',(89.5,-45.3272645584125,52.5));
#17122=CARTESIAN_POINT('Origin',(89.5,-44.3272645584125,49.8489128715187));
#17123=CARTESIAN_POINT('',(90.,-44.3272645584125,49.8489128715187));
#17124=CARTESIAN_POINT('Origin',(89.5,-32.5,52.5));
#17125=CARTESIAN_POINT('',(90.,-32.5,52.5));
#17126=CARTESIAN_POINT('Origin',(-89.5,-45.3272645584124,51.5));
#17127=CARTESIAN_POINT('',(-90.,-45.3272645584124,52.5));
#17128=CARTESIAN_POINT('Origin',(-89.5,-45.3272645584124,52.5));
#17129=CARTESIAN_POINT('',(-90.,-44.3272645584124,51.5));
#17130=CARTESIAN_POINT('Origin',(-90.,-45.3272645584124,51.5));
#17131=CARTESIAN_POINT('Origin',(-89.5,-44.3272645584124,51.5));
#17132=CARTESIAN_POINT('Origin',(-89.5,32.5,52.5));
#17133=CARTESIAN_POINT('',(-90.,32.5,52.5));
#17134=CARTESIAN_POINT('Origin',(-89.5,-44.3272645584124,49.8489128715187));
#17135=CARTESIAN_POINT('',(-90.,-44.3272645584124,49.8489128715187));
#17136=CARTESIAN_POINT('Origin',(-45.,-64.5,52.5));
#17137=CARTESIAN_POINT('',(-45.,-65.,52.5));
#17138=CARTESIAN_POINT('Origin',(-89.5,-64.5,52.));
#17139=CARTESIAN_POINT('',(-90.,-64.5,52.));
#17140=CARTESIAN_POINT('',(-89.5,-65.,52.));
#17141=CARTESIAN_POINT('Origin',(-89.5,21.7129396307488,48.1978257430375));
#17142=CARTESIAN_POINT('',(-90.,21.7129396307488,48.1978257430375));
#17143=CARTESIAN_POINT('Origin',(-90.,-44.3272645584124,48.1978257430375));
#17144=CARTESIAN_POINT('',(-90.,-44.8272645584124,48.1978257430375));
#17145=CARTESIAN_POINT('Origin',(89.5,-64.5,52.));
#17146=CARTESIAN_POINT('',(89.5,-65.,52.));
#17147=CARTESIAN_POINT('',(90.,-64.5,52.));
#17148=CARTESIAN_POINT('Origin',(-45.,-64.5,63.5));
#17149=CARTESIAN_POINT('',(-45.,-64.5,64.));
#17150=CARTESIAN_POINT('',(-45.,-65.,63.5));
#17151=CARTESIAN_POINT('Origin',(-89.5,32.5,63.5));
#17152=CARTESIAN_POINT('',(-89.5,32.5,64.));
#17153=CARTESIAN_POINT('',(-90.,32.5,63.5));
#17154=CARTESIAN_POINT('Origin',(-89.5,-21.0741207385023,43.8489128715187));
#17155=CARTESIAN_POINT('',(-90.,-21.0741207385023,43.8489128715187));
#17156=CARTESIAN_POINT('Origin',(89.5,-32.5,63.5));
#17157=CARTESIAN_POINT('',(89.5,-32.5,64.));
#17158=CARTESIAN_POINT('',(90.,-32.5,63.5));
#17159=CARTESIAN_POINT('Origin',(45.,64.5,63.5));
#17160=CARTESIAN_POINT('',(45.,64.5,64.));
#17161=CARTESIAN_POINT('',(45.,65.,63.5));
#17162=CARTESIAN_POINT('Origin',(-89.5,42.0226500362545,36.1978257430375));
#17163=CARTESIAN_POINT('',(-90.,42.0226500362545,36.1978257430375));
#17164=CARTESIAN_POINT('Origin',(-90.,-21.0741207385023,36.1978257430375));
#17165=CARTESIAN_POINT('',(-90.,-21.5741207385023,36.1978257430375));
#17166=CARTESIAN_POINT('Origin',(45.,64.5,52.5));
#17167=CARTESIAN_POINT('',(45.,65.,52.5));
#17168=CARTESIAN_POINT('Origin',(-89.5,18.5453000725091,49.8489128715187));
#17169=CARTESIAN_POINT('',(-90.,18.5453000725091,49.8489128715187));
#17170=CARTESIAN_POINT('Origin',(-45.,23.0395928638606,51.5));
#17171=CARTESIAN_POINT('',(-45.,22.6860394732673,51.1464466094067));
#17172=CARTESIAN_POINT('Origin',(-89.5,45.5673301698183,48.1978257430375));
#17173=CARTESIAN_POINT('',(-90.,45.5673301698183,48.1978257430375));
#17174=CARTESIAN_POINT('Origin',(89.5,-0.229188828587741,73.3545681300752));
#17175=CARTESIAN_POINT('',(90.,-0.229188828587741,73.3545681300752));
#17176=CARTESIAN_POINT('Origin',(-90.,24.92755355845,48.1978257430375));
#17177=CARTESIAN_POINT('',(-90.,24.92755355845,47.6978257430375));
#17178=CARTESIAN_POINT('',(-90.,25.2811069490433,48.5513791336308));
#17179=CARTESIAN_POINT('Origin',(-90.,65.,52.));
#17180=CARTESIAN_POINT('Origin',(-90.,21.8324860826741,52.));
#17181=CARTESIAN_POINT('Origin',(90.,65.,52.));
#17182=CARTESIAN_POINT('Origin',(-90.,-44.8272645584124,47.6978257430375));
#17183=CARTESIAN_POINT('Origin',(-90.,-65.,52.));
#17184=CARTESIAN_POINT('Origin',(0.,0.,64.));
#17185=CARTESIAN_POINT('Origin',(-90.,-21.5741207385023,35.6978257430375));
#17186=CARTESIAN_POINT('Origin',(-90.,26.1346603396366,47.6978257430375));
#17187=CARTESIAN_POINT('Origin',(90.,-65.,52.));
#17188=CARTESIAN_POINT('',(0.,0.,0.));
#17189=CARTESIAN_POINT('Origin',(-69.9040264336917,-84.8,3.08953555269655));
#17190=CARTESIAN_POINT('',(-104.475451921837,-84.8,2.78953555269655));
#17191=CARTESIAN_POINT('',(-104.475451921837,-84.5,3.08953555269655));
#17192=CARTESIAN_POINT('Origin',(-104.475451921837,-84.8,3.08953555269655));
#17193=CARTESIAN_POINT('',(-77.8080528673835,-84.5,3.08953555269655));
#17194=CARTESIAN_POINT('',(-69.9040264336917,-84.5,3.08953555269655));
#17195=CARTESIAN_POINT('',(-77.8080528673835,-84.8,2.78953555269655));
#17196=CARTESIAN_POINT('Origin',(-77.8080528673835,-84.8,3.08953555269655));
#17197=CARTESIAN_POINT('',(-69.9040264336917,-84.8,2.78953555269655));
#17198=CARTESIAN_POINT('Origin',(-77.8080528673835,-80.,3.08953555269655));
#17199=CARTESIAN_POINT('',(-77.8080528673835,-75.5,3.08953555269655));
#17200=CARTESIAN_POINT('',(-77.8080528673835,-75.2,2.78953555269655));
#17201=CARTESIAN_POINT('Origin',(-77.8080528673835,-75.2,3.08953555269655));
#17202=CARTESIAN_POINT('Origin',(-77.8080528673835,-80.,2.78953555269655));
#17203=CARTESIAN_POINT('Origin',(-77.8080528673835,-80.,3.08953555269655));
#17204=CARTESIAN_POINT('Origin',(-83.2377259609183,-75.2,3.08953555269655));
#17205=CARTESIAN_POINT('',(-104.475451921837,-75.5,3.08953555269655));
#17206=CARTESIAN_POINT('',(-104.475451921837,-75.2,2.78953555269655));
#17207=CARTESIAN_POINT('Origin',(-104.475451921837,-75.2,3.08953555269655));
#17208=CARTESIAN_POINT('',(-83.2377259609183,-75.2,2.78953555269655));
#17209=CARTESIAN_POINT('',(-83.2377259609183,-75.5,3.08953555269655));
#17210=CARTESIAN_POINT('Origin',(-104.475451921837,-80.,3.08953555269655));
#17211=CARTESIAN_POINT('Origin',(-104.475451921837,-80.,2.78953555269655));
#17212=CARTESIAN_POINT('Origin',(-104.475451921837,-80.,3.08953555269655));
#17213=CARTESIAN_POINT('Origin',(-77.8080528673835,-80.,10.7895355526966));
#17214=CARTESIAN_POINT('',(-77.8080528673835,-84.5,10.4895355526966));
#17215=CARTESIAN_POINT('',(-77.8080528673835,-84.5,10.7895355526966));
#17216=CARTESIAN_POINT('',(-77.8080528673835,-75.5,10.4895355526966));
#17217=CARTESIAN_POINT('Origin',(-77.8080528673835,-80.,10.4895355526966));
#17218=CARTESIAN_POINT('',(-77.8080528673835,-75.5,10.7895355526966));
#17219=CARTESIAN_POINT('Origin',(-77.8080528673835,-84.5,10.7895355526966));
#17220=CARTESIAN_POINT('',(-104.475451921837,-84.5,10.4895355526966));
#17221=CARTESIAN_POINT('',(-104.475451921837,-84.5,10.7895355526966));
#17222=CARTESIAN_POINT('',(-94.9040264336917,-84.5,10.4895355526966));
#17223=CARTESIAN_POINT('Origin',(-62.,-90.,2.78953555269655));
#17224=CARTESIAN_POINT('',(-109.7,-89.7,2.78953555269655));
#17225=CARTESIAN_POINT('',(-62.7242640687119,-89.7,2.78953555269655));
#17226=CARTESIAN_POINT('',(-74.5,-89.7,2.78953555269655));
#17227=CARTESIAN_POINT('',(-109.7,-70.3,2.78953555269655));
#17228=CARTESIAN_POINT('',(-109.7,-90.,2.78953555269655));
#17229=CARTESIAN_POINT('',(-62.7242640687119,-70.3,2.78953555269655));
#17230=CARTESIAN_POINT('',(-74.5,-70.3,2.78953555269655));
#17231=CARTESIAN_POINT('',(-62.7242640687119,-90.,2.78953555269655));
#17232=CARTESIAN_POINT('Origin',(-109.7,-70.3,2.48953555269655));
#17233=CARTESIAN_POINT('',(-109.7,-70.,3.08953555269655));
#17234=CARTESIAN_POINT('Origin',(-109.7,-70.3,3.08953555269655));
#17235=CARTESIAN_POINT('',(-110.,-70.3,2.48953555269655));
#17236=CARTESIAN_POINT('Origin',(-109.7,-70.3,2.48953555269655));
#17237=CARTESIAN_POINT('',(-110.3,-70.,2.48953555269655));
#17238=CARTESIAN_POINT('Origin',(-110.3,-70.3,2.48953555269655));
#17239=CARTESIAN_POINT('Origin',(-109.7,-70.,2.48953555269655));
#17240=CARTESIAN_POINT('Origin',(-111.7,-70.3,0.3));
#17241=CARTESIAN_POINT('',(-111.7,-70.3,0.));
#17242=CARTESIAN_POINT('',(-111.7,-70.,0.3));
#17243=CARTESIAN_POINT('Origin',(-111.7,-70.3,0.3));
#17244=CARTESIAN_POINT('',(-112.,-70.3,0.3));
#17245=CARTESIAN_POINT('Origin',(-111.7,-70.3,0.3));
#17246=CARTESIAN_POINT('Origin',(-111.7,-70.3,0.3));
#17247=CARTESIAN_POINT('Origin',(-109.7,-89.7,2.48953555269655));
#17248=CARTESIAN_POINT('',(-109.7,-90.,3.08953555269655));
#17249=CARTESIAN_POINT('',(-110.3,-90.,2.48953555269655));
#17250=CARTESIAN_POINT('Origin',(-109.7,-90.,2.48953555269655));
#17251=CARTESIAN_POINT('',(-110.,-89.7,2.48953555269655));
#17252=CARTESIAN_POINT('Origin',(-110.3,-89.7,2.48953555269655));
#17253=CARTESIAN_POINT('Origin',(-109.7,-89.7,2.48953555269655));
#17254=CARTESIAN_POINT('Origin',(-109.7,-89.7,3.08953555269655));
#17255=CARTESIAN_POINT('Origin',(-110.3,-89.7,4.09215166452241));
#17256=CARTESIAN_POINT('',(-110.,-89.7,0.));
#17257=CARTESIAN_POINT('',(-110.,-89.7,4.09215166452241));
#17258=CARTESIAN_POINT('',(-110.3,-90.,0.3));
#17259=CARTESIAN_POINT('',(-110.3,-90.,4.09215166452241));
#17260=CARTESIAN_POINT('Origin',(-110.3,-89.7,0.3));
#17261=CARTESIAN_POINT('Origin',(-62.7242640687119,-70.3,3.08953555269655));
#17262=CARTESIAN_POINT('',(-62.512132034356,-70.3,3.30166758705252));
#17263=CARTESIAN_POINT('',(-62.7242640687119,-70.,3.08953555269655));
#17264=CARTESIAN_POINT('Origin',(-62.7242640687119,-70.3,3.08953555269656));
#17265=CARTESIAN_POINT('Origin',(-62.7242640687119,-70.3,3.08953555269655));
#17266=CARTESIAN_POINT('Origin',(-62.7242640687119,-70.3,3.08953555269655));
#17267=CARTESIAN_POINT('Origin',(-111.7,-89.7,0.3));
#17268=CARTESIAN_POINT('',(-111.7,-89.7,0.));
#17269=CARTESIAN_POINT('',(-112.,-89.7,0.3));
#17270=CARTESIAN_POINT('Origin',(-111.7,-89.7,0.3));
#17271=CARTESIAN_POINT('',(-111.7,-90.,0.3));
#17272=CARTESIAN_POINT('Origin',(-111.7,-89.7,0.3));
#17273=CARTESIAN_POINT('Origin',(-111.7,-89.7,0.3));
#17274=CARTESIAN_POINT('Origin',(-98.5,-89.7,0.3));
#17275=CARTESIAN_POINT('',(-98.5,-90.,0.3));
#17276=CARTESIAN_POINT('',(-98.5,-89.7,0.));
#17277=CARTESIAN_POINT('Origin',(-111.7,-70.3,10.4895355526966));
#17278=CARTESIAN_POINT('',(-112.,-70.3,10.4895355526966));
#17279=CARTESIAN_POINT('',(-111.7,-70.,10.4895355526966));
#17280=CARTESIAN_POINT('Origin',(-111.7,-70.3,10.4895355526966));
#17281=CARTESIAN_POINT('',(-111.7,-70.3,10.7895355526966));
#17282=CARTESIAN_POINT('Origin',(-111.7,-70.3,10.4895355526966));
#17283=CARTESIAN_POINT('Origin',(-111.7,-70.3,10.4895355526966));
#17284=CARTESIAN_POINT('Origin',(-62.7242640687119,-89.7,3.08953555269655));
#17285=CARTESIAN_POINT('',(-62.512132034356,-89.7,3.30166758705252));
#17286=CARTESIAN_POINT('Origin',(-62.7242640687119,-89.7,3.08953555269655));
#17287=CARTESIAN_POINT('',(-62.7242640687119,-90.,3.08953555269655));
#17288=CARTESIAN_POINT('Origin',(-62.7242640687119,-89.7,3.08953555269655));
#17289=CARTESIAN_POINT('Origin',(-62.7242640687119,-89.7,3.08953555269655));
#17290=CARTESIAN_POINT('Origin',(-70.1242640687119,-70.3,10.4895355526966));
#17291=CARTESIAN_POINT('',(-70.1242640687119,-70.3,10.7895355526966));
#17292=CARTESIAN_POINT('',(-70.1242640687119,-70.,10.4895355526966));
#17293=CARTESIAN_POINT('Origin',(-70.1242640687119,-70.3,10.4895355526966));
#17294=CARTESIAN_POINT('',(-69.9121320343559,-70.3,10.7016675870525));
#17295=CARTESIAN_POINT('Origin',(-70.1242640687119,-70.3,10.4895355526966));
#17296=CARTESIAN_POINT('Origin',(-70.1242640687119,-70.3,10.4895355526966));
#17297=CARTESIAN_POINT('Origin',(-111.7,-89.7,10.4895355526966));
#17298=CARTESIAN_POINT('',(-112.,-89.7,10.4895355526966));
#17299=CARTESIAN_POINT('',(-111.7,-89.7,10.7895355526966));
#17300=CARTESIAN_POINT('Origin',(-111.7,-89.7,10.4895355526966));
#17301=CARTESIAN_POINT('',(-111.7,-90.,10.4895355526966));
#17302=CARTESIAN_POINT('Origin',(-111.7,-89.7,10.4895355526966));
#17303=CARTESIAN_POINT('Origin',(-111.7,-89.7,10.4895355526966));
#17304=CARTESIAN_POINT('Origin',(-111.7,-89.7,2.69738388817414));
#17305=CARTESIAN_POINT('',(-112.,-89.7,2.69738388817414));
#17306=CARTESIAN_POINT('',(-111.7,-90.,2.69738388817414));
#17307=CARTESIAN_POINT('Origin',(-70.1242640687119,-89.7,10.4895355526966));
#17308=CARTESIAN_POINT('',(-70.1242640687119,-89.7,10.7895355526966));
#17309=CARTESIAN_POINT('',(-69.9121320343559,-89.7,10.7016675870525));
#17310=CARTESIAN_POINT('Origin',(-70.1242640687119,-89.7,10.4895355526966));
#17311=CARTESIAN_POINT('',(-70.1242640687119,-90.,10.4895355526966));
#17312=CARTESIAN_POINT('Origin',(-70.1242640687119,-89.7,10.4895355526966));
#17313=CARTESIAN_POINT('Origin',(-70.1242640687119,-89.7,10.4895355526966));
#17314=CARTESIAN_POINT('Origin',(-99.5,-89.7,10.4895355526966));
#17315=CARTESIAN_POINT('',(-99.5,-90.,10.4895355526966));
#17316=CARTESIAN_POINT('',(-99.5,-89.7,10.7895355526966));
#17317=CARTESIAN_POINT('Origin',(-73.1134400902689,-89.7,13.4787115742535));
#17318=CARTESIAN_POINT('',(-73.1134400902689,-90.,13.4787115742535));
#17319=CARTESIAN_POINT('',(-72.9013080559129,-89.7,13.6908436086095));
#17320=CARTESIAN_POINT('Origin',(-70.1242640687119,-90.,10.4895355526966));
#17321=CARTESIAN_POINT('',(-70.1242640687119,-90.,10.7895355526966));
#17322=CARTESIAN_POINT('',(-69.9121320343559,-90.,10.7016675870525));
#17323=CARTESIAN_POINT('Origin',(-111.7,-90.,10.4895355526966));
#17324=CARTESIAN_POINT('',(-112.,-90.,10.4895355526966));
#17325=CARTESIAN_POINT('',(-111.7,-90.,10.7895355526966));
#17326=CARTESIAN_POINT('Origin',(-73.1134400902689,-70.3,13.4787115742535));
#17327=CARTESIAN_POINT('',(-73.1134400902689,-70.,13.4787115742535));
#17328=CARTESIAN_POINT('',(-72.9013080559129,-70.3,13.6908436086095));
#17329=CARTESIAN_POINT('Origin',(-99.5,-70.3,10.4895355526966));
#17330=CARTESIAN_POINT('',(-99.5,-70.,10.4895355526966));
#17331=CARTESIAN_POINT('',(-99.5,-70.3,10.7895355526966));
#17332=CARTESIAN_POINT('Origin',(-74.5,-89.7,3.08953555269655));
#17333=CARTESIAN_POINT('',(-74.5,-90.,3.08953555269655));
#17334=CARTESIAN_POINT('Origin',(-62.7242640687119,-90.,3.08953555269655));
#17335=CARTESIAN_POINT('',(-62.512132034356,-90.,3.30166758705252));
#17336=CARTESIAN_POINT('Origin',(-111.7,-70.3,2.69738388817414));
#17337=CARTESIAN_POINT('',(-111.7,-70.,2.69738388817414));
#17338=CARTESIAN_POINT('',(-112.,-70.3,2.69738388817414));
#17339=CARTESIAN_POINT('Origin',(-111.7,-90.,0.3));
#17340=CARTESIAN_POINT('',(-111.7,-90.,0.));
#17341=CARTESIAN_POINT('',(-112.,-90.,0.3));
#17342=CARTESIAN_POINT('Origin',(-74.5,-70.3,3.08953555269655));
#17343=CARTESIAN_POINT('',(-74.5,-70.,3.08953555269655));
#17344=CARTESIAN_POINT('Origin',(-109.7,-90.,2.48953555269655));
#17345=CARTESIAN_POINT('',(-110.,-90.,2.48953555269655));
#17346=CARTESIAN_POINT('Origin',(-98.5,-70.3,0.3));
#17347=CARTESIAN_POINT('',(-110.,-70.3,0.));
#17348=CARTESIAN_POINT('',(-98.5,-70.3,0.));
#17349=CARTESIAN_POINT('',(-110.3,-70.,0.3));
#17350=CARTESIAN_POINT('',(-98.5,-70.,0.3));
#17351=CARTESIAN_POINT('Origin',(-110.3,-70.3,0.3));
#17352=CARTESIAN_POINT('Origin',(-110.3,-70.3,4.09215166452241));
#17353=CARTESIAN_POINT('',(-110.3,-70.,4.09215166452241));
#17354=CARTESIAN_POINT('',(-110.,-70.3,4.09215166452241));
#17355=CARTESIAN_POINT('Origin',(-110.,-90.,2.78953555269655));
#17356=CARTESIAN_POINT('',(-110.,-90.,0.));
#17357=CARTESIAN_POINT('Origin',(-87.,-90.,5.39476777634828));
#17358=CARTESIAN_POINT('Origin',(-112.,-90.,0.));
#17359=CARTESIAN_POINT('Origin',(-112.,-90.,10.7895355526966));
#17360=CARTESIAN_POINT('',(-104.475451921837,-84.8,10.7895355526966));
#17361=CARTESIAN_POINT('',(-77.8080528673835,-84.8,10.7895355526966));
#17362=CARTESIAN_POINT('',(-94.9040264336917,-84.8,10.7895355526966));
#17363=CARTESIAN_POINT('',(-104.475451921837,-75.2,10.7895355526966));
#17364=CARTESIAN_POINT('Origin',(-104.475451921837,-80.,10.7895355526966));
#17365=CARTESIAN_POINT('',(-77.8080528673835,-75.2,10.7895355526966));
#17366=CARTESIAN_POINT('',(-108.237725960918,-75.2,10.7895355526966));
#17367=CARTESIAN_POINT('Origin',(-77.8080528673835,-80.,10.7895355526966));
#17368=CARTESIAN_POINT('Origin',(-70.,-90.,10.7895355526965));
#17369=CARTESIAN_POINT('Origin',(-87.,-70.,5.39476777634828));
#17370=CARTESIAN_POINT('Origin',(-94.9040264336917,-84.8,10.4895355526966));
#17371=CARTESIAN_POINT('Origin',(-77.8080528673835,-84.8,10.4895355526966));
#17372=CARTESIAN_POINT('Origin',(-104.475451921837,-84.8,10.4895355526966));
#17373=CARTESIAN_POINT('Origin',(-104.475451921837,-80.,10.4895355526966));
#17374=CARTESIAN_POINT('',(-104.475451921837,-75.5,10.4895355526966));
#17375=CARTESIAN_POINT('Origin',(-104.475451921837,-75.2,10.4895355526966));
#17376=CARTESIAN_POINT('Origin',(-104.475451921837,-80.,10.4895355526966));
#17377=CARTESIAN_POINT('Origin',(-108.237725960918,-75.2,10.4895355526966));
#17378=CARTESIAN_POINT('Origin',(-77.8080528673835,-75.2,10.4895355526966));
#17379=CARTESIAN_POINT('',(-108.237725960918,-75.5,10.4895355526966));
#17380=CARTESIAN_POINT('Origin',(-77.8080528673835,-80.,10.4895355526966));
#17381=CARTESIAN_POINT('Origin',(-104.475451921837,-80.,10.7895355526966));
#17382=CARTESIAN_POINT('',(-104.475451921837,-75.5,10.7895355526966));
#17383=CARTESIAN_POINT('Origin',(-104.475451921837,-75.5,10.7895355526966));
#17384=CARTESIAN_POINT('Origin',(-110.,-90.,0.));
#17385=CARTESIAN_POINT('',(0.,0.,0.));
#17386=CARTESIAN_POINT('Origin',(-115.,1.77635683940025E-14,49.8489128715187));
#17387=CARTESIAN_POINT('',(-115.,8.00000000000002,49.8489128715187));
#17388=CARTESIAN_POINT('Origin',(-115.,1.77635683940025E-14,49.8489128715187));
#17389=CARTESIAN_POINT('',(-115.,7.50000000000002,49.8489128715187));
#17390=CARTESIAN_POINT('Origin',(-115.,1.77635683940025E-14,49.8489128715187));
#17391=CARTESIAN_POINT('Origin',(-134.5,5.32907051820075E-14,49.8489128715187));
#17392=CARTESIAN_POINT('',(-135.,8.00000000000004,49.8489128715187));
#17393=CARTESIAN_POINT('Origin',(-135.,5.32907051820075E-14,49.8489128715187));
#17394=CARTESIAN_POINT('',(-134.,9.00000000000004,49.8489128715187));
#17395=CARTESIAN_POINT('',(-134.5,8.50000000000005,49.8489128715187));
#17396=CARTESIAN_POINT('Origin',(-134.,5.32907051820075E-14,49.8489128715187));
#17397=CARTESIAN_POINT('Origin',(-115.,1.77635683940025E-14,49.8489128715187));
#17398=CARTESIAN_POINT('',(-116.,9.00000000000002,49.8489128715187));
#17399=CARTESIAN_POINT('',(-115.,9.00000000000002,49.8489128715187));
#17400=CARTESIAN_POINT('Origin',(-116.,1.77635683940025E-14,49.8489128715187));
#17401=CARTESIAN_POINT('Origin',(-135.,5.32907051820075E-14,49.8489128715187));
#17402=CARTESIAN_POINT('Origin',(-115.5,1.77635683940025E-14,49.8489128715187));
#17403=CARTESIAN_POINT('',(-115.5,8.50000000000002,49.8489128715187));
#17404=CARTESIAN_POINT('Origin',(-90.,1.77635683940025E-14,49.8489128715187));
#17405=CARTESIAN_POINT('',(-90.,7.50000000000002,49.8489128715187));
#17406=CARTESIAN_POINT('',(-90.,7.50000000000002,49.8489128715187));
#17407=CARTESIAN_POINT('Origin',(-90.,1.77635683940025E-14,49.8489128715187));
#17408=CARTESIAN_POINT('Origin',(-90.,1.77635683940025E-14,49.8489128715187));
#17409=CARTESIAN_POINT('',(0.,0.,0.));
#17410=CARTESIAN_POINT('Origin',(69.9040264336917,-84.8,3.08953555269655));
#17411=CARTESIAN_POINT('',(104.475451921837,-84.8,2.78953555269655));
#17412=CARTESIAN_POINT('',(104.475451921837,-84.5,3.08953555269655));
#17413=CARTESIAN_POINT('Origin',(104.475451921837,-84.8,3.08953555269655));
#17414=CARTESIAN_POINT('',(77.8080528673835,-84.8,2.78953555269655));
#17415=CARTESIAN_POINT('',(69.9040264336917,-84.8,2.78953555269655));
#17416=CARTESIAN_POINT('',(77.8080528673835,-84.5,3.08953555269655));
#17417=CARTESIAN_POINT('Origin',(77.8080528673835,-84.8,3.08953555269655));
#17418=CARTESIAN_POINT('',(69.9040264336917,-84.5,3.08953555269655));
#17419=CARTESIAN_POINT('Origin',(77.8080528673835,-80.,3.08953555269655));
#17420=CARTESIAN_POINT('',(77.8080528673835,-75.5,3.08953555269655));
#17421=CARTESIAN_POINT('',(77.8080528673835,-75.2,2.78953555269655));
#17422=CARTESIAN_POINT('Origin',(77.8080528673835,-75.2,3.08953555269655));
#17423=CARTESIAN_POINT('Origin',(77.8080528673835,-80.,3.08953555269655));
#17424=CARTESIAN_POINT('Origin',(77.8080528673835,-80.,2.78953555269655));
#17425=CARTESIAN_POINT('Origin',(83.2377259609183,-75.2,3.08953555269655));
#17426=CARTESIAN_POINT('',(104.475451921837,-75.5,3.08953555269655));
#17427=CARTESIAN_POINT('',(104.475451921837,-75.2,2.78953555269655));
#17428=CARTESIAN_POINT('Origin',(104.475451921837,-75.2,3.08953555269655));
#17429=CARTESIAN_POINT('',(83.2377259609183,-75.5,3.08953555269655));
#17430=CARTESIAN_POINT('',(83.2377259609183,-75.2,2.78953555269655));
#17431=CARTESIAN_POINT('Origin',(104.475451921837,-80.,3.08953555269655));
#17432=CARTESIAN_POINT('Origin',(104.475451921837,-80.,3.08953555269655));
#17433=CARTESIAN_POINT('Origin',(104.475451921837,-80.,2.78953555269655));
#17434=CARTESIAN_POINT('Origin',(77.8080528673835,-80.,10.7895355526966));
#17435=CARTESIAN_POINT('',(77.8080528673835,-75.5,10.4895355526966));
#17436=CARTESIAN_POINT('',(77.8080528673835,-75.5,10.7895355526966));
#17437=CARTESIAN_POINT('',(77.8080528673835,-84.5,10.4895355526966));
#17438=CARTESIAN_POINT('Origin',(77.8080528673835,-80.,10.4895355526966));
#17439=CARTESIAN_POINT('',(77.8080528673835,-84.5,10.7895355526966));
#17440=CARTESIAN_POINT('Origin',(77.8080528673835,-84.5,10.7895355526966));
#17441=CARTESIAN_POINT('',(104.475451921837,-84.5,10.4895355526966));
#17442=CARTESIAN_POINT('',(94.9040264336917,-84.5,10.4895355526966));
#17443=CARTESIAN_POINT('',(104.475451921837,-84.5,10.7895355526966));
#17444=CARTESIAN_POINT('Origin',(62.,-90.,2.78953555269655));
#17445=CARTESIAN_POINT('',(109.7,-89.7,2.78953555269655));
#17446=CARTESIAN_POINT('',(62.7242640687119,-89.7,2.78953555269655));
#17447=CARTESIAN_POINT('',(74.5,-89.7,2.78953555269655));
#17448=CARTESIAN_POINT('',(62.7242640687119,-70.3,2.78953555269655));
#17449=CARTESIAN_POINT('',(62.7242640687119,-90.,2.78953555269655));
#17450=CARTESIAN_POINT('',(109.7,-70.3,2.78953555269655));
#17451=CARTESIAN_POINT('',(74.5,-70.3,2.78953555269655));
#17452=CARTESIAN_POINT('',(109.7,-90.,2.78953555269655));
#17453=CARTESIAN_POINT('Origin',(109.7,-70.3,2.48953555269655));
#17454=CARTESIAN_POINT('',(109.7,-70.,3.08953555269655));
#17455=CARTESIAN_POINT('Origin',(109.7,-70.3,3.08953555269655));
#17456=CARTESIAN_POINT('',(110.3,-70.,2.48953555269655));
#17457=CARTESIAN_POINT('Origin',(109.7,-70.,2.48953555269655));
#17458=CARTESIAN_POINT('',(110.,-70.3,2.48953555269655));
#17459=CARTESIAN_POINT('Origin',(110.3,-70.3,2.48953555269655));
#17460=CARTESIAN_POINT('Origin',(109.7,-70.3,2.48953555269655));
#17461=CARTESIAN_POINT('Origin',(111.7,-70.3,0.3));
#17462=CARTESIAN_POINT('',(111.7,-70.3,0.));
#17463=CARTESIAN_POINT('',(111.7,-70.,0.3));
#17464=CARTESIAN_POINT('Origin',(111.7,-70.3,0.3));
#17465=CARTESIAN_POINT('',(112.,-70.3,0.3));
#17466=CARTESIAN_POINT('Origin',(111.7,-70.3,0.3));
#17467=CARTESIAN_POINT('Origin',(111.7,-70.3,0.3));
#17468=CARTESIAN_POINT('Origin',(109.7,-89.7,2.48953555269655));
#17469=CARTESIAN_POINT('',(109.7,-90.,3.08953555269655));
#17470=CARTESIAN_POINT('',(110.3,-90.,2.48953555269655));
#17471=CARTESIAN_POINT('Origin',(109.7,-90.,2.48953555269655));
#17472=CARTESIAN_POINT('Origin',(109.7,-89.7,3.08953555269655));
#17473=CARTESIAN_POINT('',(110.,-89.7,2.48953555269655));
#17474=CARTESIAN_POINT('Origin',(109.7,-89.7,2.48953555269655));
#17475=CARTESIAN_POINT('Origin',(110.3,-89.7,2.48953555269655));
#17476=CARTESIAN_POINT('Origin',(110.3,-89.7,4.09215166452241));
#17477=CARTESIAN_POINT('',(110.,-89.7,0.));
#17478=CARTESIAN_POINT('',(110.,-89.7,4.09215166452241));
#17479=CARTESIAN_POINT('',(110.3,-90.,0.3));
#17480=CARTESIAN_POINT('Origin',(110.3,-89.7,0.3));
#17481=CARTESIAN_POINT('',(110.3,-90.,4.09215166452241));
#17482=CARTESIAN_POINT('Origin',(62.7242640687119,-70.3,3.08953555269655));
#17483=CARTESIAN_POINT('',(62.512132034356,-70.3,3.30166758705252));
#17484=CARTESIAN_POINT('',(62.7242640687119,-70.,3.08953555269655));
#17485=CARTESIAN_POINT('Origin',(62.7242640687119,-70.3,3.08953555269656));
#17486=CARTESIAN_POINT('Origin',(62.7242640687119,-70.3,3.08953555269655));
#17487=CARTESIAN_POINT('Origin',(62.7242640687119,-70.3,3.08953555269655));
#17488=CARTESIAN_POINT('Origin',(111.7,-89.7,0.3));
#17489=CARTESIAN_POINT('',(111.7,-89.7,0.));
#17490=CARTESIAN_POINT('',(112.,-89.7,0.3));
#17491=CARTESIAN_POINT('Origin',(111.7,-89.7,0.3));
#17492=CARTESIAN_POINT('',(111.7,-90.,0.3));
#17493=CARTESIAN_POINT('Origin',(111.7,-89.7,0.3));
#17494=CARTESIAN_POINT('Origin',(111.7,-89.7,0.3));
#17495=CARTESIAN_POINT('Origin',(98.5,-89.7,0.3));
#17496=CARTESIAN_POINT('',(98.5,-90.,0.3));
#17497=CARTESIAN_POINT('',(98.5,-89.7,0.));
#17498=CARTESIAN_POINT('Origin',(111.7,-70.3,10.4895355526966));
#17499=CARTESIAN_POINT('',(112.,-70.3,10.4895355526966));
#17500=CARTESIAN_POINT('',(111.7,-70.,10.4895355526966));
#17501=CARTESIAN_POINT('Origin',(111.7,-70.3,10.4895355526966));
#17502=CARTESIAN_POINT('',(111.7,-70.3,10.7895355526966));
#17503=CARTESIAN_POINT('Origin',(111.7,-70.3,10.4895355526966));
#17504=CARTESIAN_POINT('Origin',(111.7,-70.3,10.4895355526966));
#17505=CARTESIAN_POINT('Origin',(62.7242640687119,-89.7,3.08953555269655));
#17506=CARTESIAN_POINT('',(62.512132034356,-89.7,3.30166758705252));
#17507=CARTESIAN_POINT('Origin',(62.7242640687119,-89.7,3.08953555269655));
#17508=CARTESIAN_POINT('',(62.7242640687119,-90.,3.08953555269655));
#17509=CARTESIAN_POINT('Origin',(62.7242640687119,-89.7,3.08953555269655));
#17510=CARTESIAN_POINT('Origin',(62.7242640687119,-89.7,3.08953555269655));
#17511=CARTESIAN_POINT('Origin',(70.1242640687119,-70.3,10.4895355526966));
#17512=CARTESIAN_POINT('',(70.1242640687119,-70.3,10.7895355526966));
#17513=CARTESIAN_POINT('',(70.1242640687119,-70.,10.4895355526966));
#17514=CARTESIAN_POINT('Origin',(70.1242640687119,-70.3,10.4895355526966));
#17515=CARTESIAN_POINT('',(69.9121320343559,-70.3,10.7016675870525));
#17516=CARTESIAN_POINT('Origin',(70.1242640687119,-70.3,10.4895355526966));
#17517=CARTESIAN_POINT('Origin',(70.1242640687119,-70.3,10.4895355526966));
#17518=CARTESIAN_POINT('Origin',(111.7,-89.7,10.4895355526966));
#17519=CARTESIAN_POINT('',(112.,-89.7,10.4895355526966));
#17520=CARTESIAN_POINT('',(111.7,-89.7,10.7895355526966));
#17521=CARTESIAN_POINT('Origin',(111.7,-89.7,10.4895355526966));
#17522=CARTESIAN_POINT('',(111.7,-90.,10.4895355526966));
#17523=CARTESIAN_POINT('Origin',(111.7,-89.7,10.4895355526966));
#17524=CARTESIAN_POINT('Origin',(111.7,-89.7,10.4895355526966));
#17525=CARTESIAN_POINT('Origin',(111.7,-89.7,2.69738388817414));
#17526=CARTESIAN_POINT('',(111.7,-90.,2.69738388817414));
#17527=CARTESIAN_POINT('',(112.,-89.7,2.69738388817414));
#17528=CARTESIAN_POINT('Origin',(70.1242640687119,-89.7,10.4895355526966));
#17529=CARTESIAN_POINT('',(70.1242640687119,-89.7,10.7895355526966));
#17530=CARTESIAN_POINT('',(69.9121320343559,-89.7,10.7016675870525));
#17531=CARTESIAN_POINT('Origin',(70.1242640687119,-89.7,10.4895355526966));
#17532=CARTESIAN_POINT('',(70.1242640687119,-90.,10.4895355526966));
#17533=CARTESIAN_POINT('Origin',(70.1242640687119,-89.7,10.4895355526966));
#17534=CARTESIAN_POINT('Origin',(70.1242640687119,-89.7,10.4895355526966));
#17535=CARTESIAN_POINT('Origin',(99.5,-89.7,10.4895355526966));
#17536=CARTESIAN_POINT('',(99.5,-89.7,10.7895355526966));
#17537=CARTESIAN_POINT('',(99.5,-90.,10.4895355526966));
#17538=CARTESIAN_POINT('Origin',(73.1134400902689,-89.7,13.4787115742535));
#17539=CARTESIAN_POINT('',(72.9013080559129,-89.7,13.6908436086095));
#17540=CARTESIAN_POINT('',(73.1134400902689,-90.,13.4787115742535));
#17541=CARTESIAN_POINT('Origin',(70.1242640687119,-90.,10.4895355526966));
#17542=CARTESIAN_POINT('',(69.9121320343559,-90.,10.7016675870525));
#17543=CARTESIAN_POINT('',(70.1242640687119,-90.,10.7895355526966));
#17544=CARTESIAN_POINT('Origin',(111.7,-90.,10.4895355526966));
#17545=CARTESIAN_POINT('',(111.7,-90.,10.7895355526966));
#17546=CARTESIAN_POINT('',(112.,-90.,10.4895355526966));
#17547=CARTESIAN_POINT('Origin',(73.1134400902689,-70.3,13.4787115742535));
#17548=CARTESIAN_POINT('',(72.9013080559129,-70.3,13.6908436086095));
#17549=CARTESIAN_POINT('',(73.1134400902689,-70.,13.4787115742535));
#17550=CARTESIAN_POINT('Origin',(99.5,-70.3,10.4895355526966));
#17551=CARTESIAN_POINT('',(99.5,-70.3,10.7895355526966));
#17552=CARTESIAN_POINT('',(99.5,-70.,10.4895355526966));
#17553=CARTESIAN_POINT('Origin',(74.5,-89.7,3.08953555269655));
#17554=CARTESIAN_POINT('',(74.5,-90.,3.08953555269655));
#17555=CARTESIAN_POINT('Origin',(62.7242640687119,-90.,3.08953555269655));
#17556=CARTESIAN_POINT('',(62.512132034356,-90.,3.30166758705252));
#17557=CARTESIAN_POINT('Origin',(111.7,-70.3,2.69738388817414));
#17558=CARTESIAN_POINT('',(112.,-70.3,2.69738388817414));
#17559=CARTESIAN_POINT('',(111.7,-70.,2.69738388817414));
#17560=CARTESIAN_POINT('Origin',(111.7,-90.,0.3));
#17561=CARTESIAN_POINT('',(112.,-90.,0.3));
#17562=CARTESIAN_POINT('',(111.7,-90.,0.));
#17563=CARTESIAN_POINT('Origin',(74.5,-70.3,3.08953555269655));
#17564=CARTESIAN_POINT('',(74.5,-70.,3.08953555269655));
#17565=CARTESIAN_POINT('Origin',(109.7,-90.,2.48953555269655));
#17566=CARTESIAN_POINT('',(110.,-90.,2.48953555269655));
#17567=CARTESIAN_POINT('Origin',(98.5,-70.3,0.3));
#17568=CARTESIAN_POINT('',(110.,-70.3,0.));
#17569=CARTESIAN_POINT('',(98.5,-70.3,0.));
#17570=CARTESIAN_POINT('',(110.3,-70.,0.3));
#17571=CARTESIAN_POINT('Origin',(110.3,-70.3,0.3));
#17572=CARTESIAN_POINT('',(98.5,-70.,0.3));
#17573=CARTESIAN_POINT('Origin',(110.3,-70.3,4.09215166452241));
#17574=CARTESIAN_POINT('',(110.3,-70.,4.09215166452241));
#17575=CARTESIAN_POINT('',(110.,-70.3,4.09215166452241));
#17576=CARTESIAN_POINT('Origin',(110.,-90.,2.78953555269655));
#17577=CARTESIAN_POINT('',(110.,-90.,0.));
#17578=CARTESIAN_POINT('Origin',(87.,-90.,5.39476777634828));
#17579=CARTESIAN_POINT('Origin',(112.,-90.,0.));
#17580=CARTESIAN_POINT('Origin',(112.,-90.,10.7895355526966));
#17581=CARTESIAN_POINT('',(104.475451921837,-84.8,10.7895355526966));
#17582=CARTESIAN_POINT('',(77.8080528673835,-84.8,10.7895355526966));
#17583=CARTESIAN_POINT('',(94.9040264336917,-84.8,10.7895355526966));
#17584=CARTESIAN_POINT('',(77.8080528673835,-75.2,10.7895355526966));
#17585=CARTESIAN_POINT('Origin',(77.8080528673835,-80.,10.7895355526966));
#17586=CARTESIAN_POINT('',(104.475451921837,-75.2,10.7895355526966));
#17587=CARTESIAN_POINT('',(108.237725960918,-75.2,10.7895355526966));
#17588=CARTESIAN_POINT('Origin',(104.475451921837,-80.,10.7895355526966));
#17589=CARTESIAN_POINT('Origin',(70.,-90.,10.7895355526965));
#17590=CARTESIAN_POINT('Origin',(87.,-70.,5.39476777634828));
#17591=CARTESIAN_POINT('Origin',(94.9040264336917,-84.8,10.4895355526966));
#17592=CARTESIAN_POINT('Origin',(77.8080528673835,-84.8,10.4895355526966));
#17593=CARTESIAN_POINT('Origin',(104.475451921837,-84.8,10.4895355526966));
#17594=CARTESIAN_POINT('Origin',(104.475451921837,-80.,10.4895355526966));
#17595=CARTESIAN_POINT('',(104.475451921837,-75.5,10.4895355526966));
#17596=CARTESIAN_POINT('Origin',(104.475451921837,-75.2,10.4895355526966));
#17597=CARTESIAN_POINT('Origin',(104.475451921837,-80.,10.4895355526966));
#17598=CARTESIAN_POINT('Origin',(108.237725960918,-75.2,10.4895355526966));
#17599=CARTESIAN_POINT('Origin',(77.8080528673835,-75.2,10.4895355526966));
#17600=CARTESIAN_POINT('',(108.237725960918,-75.5,10.4895355526966));
#17601=CARTESIAN_POINT('Origin',(77.8080528673835,-80.,10.4895355526966));
#17602=CARTESIAN_POINT('Origin',(104.475451921837,-80.,10.7895355526966));
#17603=CARTESIAN_POINT('',(104.475451921837,-75.5,10.7895355526966));
#17604=CARTESIAN_POINT('Origin',(104.475451921837,-75.5,10.7895355526966));
#17605=CARTESIAN_POINT('Origin',(110.,-90.,0.));
#17606=CARTESIAN_POINT('',(0.,0.,0.));
#17607=CARTESIAN_POINT('Origin',(69.9040264336917,64.8,3.08953555269655));
#17608=CARTESIAN_POINT('',(104.475451921837,64.8,2.78953555269655));
#17609=CARTESIAN_POINT('',(104.475451921837,64.5,3.08953555269655));
#17610=CARTESIAN_POINT('Origin',(104.475451921837,64.8,3.08953555269655));
#17611=CARTESIAN_POINT('',(77.8080528673835,64.5,3.08953555269655));
#17612=CARTESIAN_POINT('',(69.9040264336917,64.5,3.08953555269655));
#17613=CARTESIAN_POINT('',(77.8080528673835,64.8,2.78953555269655));
#17614=CARTESIAN_POINT('Origin',(77.8080528673835,64.8,3.08953555269655));
#17615=CARTESIAN_POINT('',(69.9040264336917,64.8,2.78953555269655));
#17616=CARTESIAN_POINT('Origin',(77.8080528673835,60.,3.08953555269655));
#17617=CARTESIAN_POINT('',(77.8080528673835,55.5,3.08953555269655));
#17618=CARTESIAN_POINT('',(77.8080528673835,55.2,2.78953555269655));
#17619=CARTESIAN_POINT('Origin',(77.8080528673835,55.2,3.08953555269655));
#17620=CARTESIAN_POINT('Origin',(77.8080528673835,60.,2.78953555269655));
#17621=CARTESIAN_POINT('Origin',(77.8080528673835,60.,3.08953555269655));
#17622=CARTESIAN_POINT('Origin',(83.2377259609183,55.2,3.08953555269655));
#17623=CARTESIAN_POINT('',(104.475451921837,55.5,3.08953555269655));
#17624=CARTESIAN_POINT('',(104.475451921837,55.2,2.78953555269655));
#17625=CARTESIAN_POINT('Origin',(104.475451921837,55.2,3.08953555269655));
#17626=CARTESIAN_POINT('',(83.2377259609183,55.2,2.78953555269655));
#17627=CARTESIAN_POINT('',(83.2377259609183,55.5,3.08953555269655));
#17628=CARTESIAN_POINT('Origin',(104.475451921837,60.,3.08953555269655));
#17629=CARTESIAN_POINT('Origin',(104.475451921837,60.,2.78953555269655));
#17630=CARTESIAN_POINT('Origin',(104.475451921837,60.,3.08953555269655));
#17631=CARTESIAN_POINT('Origin',(77.8080528673835,60.,10.7895355526966));
#17632=CARTESIAN_POINT('',(77.8080528673835,64.5,10.4895355526966));
#17633=CARTESIAN_POINT('',(77.8080528673835,64.5,10.7895355526966));
#17634=CARTESIAN_POINT('',(77.8080528673835,55.5,10.4895355526966));
#17635=CARTESIAN_POINT('Origin',(77.8080528673835,60.,10.4895355526966));
#17636=CARTESIAN_POINT('',(77.8080528673835,55.5,10.7895355526966));
#17637=CARTESIAN_POINT('Origin',(77.8080528673835,64.5,10.7895355526966));
#17638=CARTESIAN_POINT('',(104.475451921837,64.5,10.4895355526966));
#17639=CARTESIAN_POINT('',(104.475451921837,64.5,10.7895355526966));
#17640=CARTESIAN_POINT('',(94.9040264336917,64.5,10.4895355526966));
#17641=CARTESIAN_POINT('Origin',(62.,70.,2.78953555269655));
#17642=CARTESIAN_POINT('',(109.7,69.7,2.78953555269655));
#17643=CARTESIAN_POINT('',(62.7242640687119,69.7,2.78953555269655));
#17644=CARTESIAN_POINT('',(74.5,69.7,2.78953555269655));
#17645=CARTESIAN_POINT('',(109.7,50.3,2.78953555269655));
#17646=CARTESIAN_POINT('',(109.7,70.,2.78953555269655));
#17647=CARTESIAN_POINT('',(62.7242640687119,50.3,2.78953555269655));
#17648=CARTESIAN_POINT('',(74.5,50.3,2.78953555269655));
#17649=CARTESIAN_POINT('',(62.7242640687119,70.,2.78953555269655));
#17650=CARTESIAN_POINT('Origin',(109.7,50.3,2.48953555269655));
#17651=CARTESIAN_POINT('',(109.7,50.,3.08953555269655));
#17652=CARTESIAN_POINT('Origin',(109.7,50.3,3.08953555269655));
#17653=CARTESIAN_POINT('',(110.,50.3,2.48953555269655));
#17654=CARTESIAN_POINT('Origin',(109.7,50.3,2.48953555269655));
#17655=CARTESIAN_POINT('',(110.3,50.,2.48953555269655));
#17656=CARTESIAN_POINT('Origin',(110.3,50.3,2.48953555269655));
#17657=CARTESIAN_POINT('Origin',(109.7,50.,2.48953555269655));
#17658=CARTESIAN_POINT('Origin',(111.7,50.3,0.3));
#17659=CARTESIAN_POINT('',(111.7,50.3,0.));
#17660=CARTESIAN_POINT('',(111.7,50.,0.3));
#17661=CARTESIAN_POINT('Origin',(111.7,50.3,0.3));
#17662=CARTESIAN_POINT('',(112.,50.3,0.3));
#17663=CARTESIAN_POINT('Origin',(111.7,50.3,0.3));
#17664=CARTESIAN_POINT('Origin',(111.7,50.3,0.3));
#17665=CARTESIAN_POINT('Origin',(109.7,69.7,2.48953555269655));
#17666=CARTESIAN_POINT('',(109.7,70.,3.08953555269655));
#17667=CARTESIAN_POINT('',(110.3,70.,2.48953555269655));
#17668=CARTESIAN_POINT('Origin',(109.7,70.,2.48953555269655));
#17669=CARTESIAN_POINT('',(110.,69.7,2.48953555269655));
#17670=CARTESIAN_POINT('Origin',(110.3,69.7,2.48953555269655));
#17671=CARTESIAN_POINT('Origin',(109.7,69.7,2.48953555269655));
#17672=CARTESIAN_POINT('Origin',(109.7,69.7,3.08953555269655));
#17673=CARTESIAN_POINT('Origin',(110.3,69.7,4.09215166452241));
#17674=CARTESIAN_POINT('',(110.,69.7,0.));
#17675=CARTESIAN_POINT('',(110.,69.7,4.09215166452241));
#17676=CARTESIAN_POINT('',(110.3,70.,0.3));
#17677=CARTESIAN_POINT('',(110.3,70.,4.09215166452241));
#17678=CARTESIAN_POINT('Origin',(110.3,69.7,0.3));
#17679=CARTESIAN_POINT('Origin',(62.7242640687119,50.3,3.08953555269655));
#17680=CARTESIAN_POINT('',(62.512132034356,50.3,3.30166758705252));
#17681=CARTESIAN_POINT('',(62.7242640687119,50.,3.08953555269655));
#17682=CARTESIAN_POINT('Origin',(62.7242640687119,50.3,3.08953555269656));
#17683=CARTESIAN_POINT('Origin',(62.7242640687119,50.3,3.08953555269655));
#17684=CARTESIAN_POINT('Origin',(62.7242640687119,50.3,3.08953555269655));
#17685=CARTESIAN_POINT('Origin',(111.7,69.7,0.3));
#17686=CARTESIAN_POINT('',(111.7,69.7,0.));
#17687=CARTESIAN_POINT('',(112.,69.7,0.3));
#17688=CARTESIAN_POINT('Origin',(111.7,69.7,0.3));
#17689=CARTESIAN_POINT('',(111.7,70.,0.3));
#17690=CARTESIAN_POINT('Origin',(111.7,69.7,0.3));
#17691=CARTESIAN_POINT('Origin',(111.7,69.7,0.3));
#17692=CARTESIAN_POINT('Origin',(98.5,69.7,0.3));
#17693=CARTESIAN_POINT('',(98.5,70.,0.3));
#17694=CARTESIAN_POINT('',(98.5,69.7,0.));
#17695=CARTESIAN_POINT('Origin',(111.7,50.3,10.4895355526966));
#17696=CARTESIAN_POINT('',(112.,50.3,10.4895355526966));
#17697=CARTESIAN_POINT('',(111.7,50.,10.4895355526966));
#17698=CARTESIAN_POINT('Origin',(111.7,50.3,10.4895355526966));
#17699=CARTESIAN_POINT('',(111.7,50.3,10.7895355526966));
#17700=CARTESIAN_POINT('Origin',(111.7,50.3,10.4895355526966));
#17701=CARTESIAN_POINT('Origin',(111.7,50.3,10.4895355526966));
#17702=CARTESIAN_POINT('Origin',(62.7242640687119,69.7,3.08953555269655));
#17703=CARTESIAN_POINT('',(62.512132034356,69.7,3.30166758705252));
#17704=CARTESIAN_POINT('Origin',(62.7242640687119,69.7,3.08953555269655));
#17705=CARTESIAN_POINT('',(62.7242640687119,70.,3.08953555269655));
#17706=CARTESIAN_POINT('Origin',(62.7242640687119,69.7,3.08953555269655));
#17707=CARTESIAN_POINT('Origin',(62.7242640687119,69.7,3.08953555269655));
#17708=CARTESIAN_POINT('Origin',(70.1242640687119,50.3,10.4895355526966));
#17709=CARTESIAN_POINT('',(70.1242640687119,50.3,10.7895355526966));
#17710=CARTESIAN_POINT('',(70.1242640687119,50.,10.4895355526966));
#17711=CARTESIAN_POINT('Origin',(70.1242640687119,50.3,10.4895355526966));
#17712=CARTESIAN_POINT('',(69.9121320343559,50.3,10.7016675870525));
#17713=CARTESIAN_POINT('Origin',(70.1242640687119,50.3,10.4895355526966));
#17714=CARTESIAN_POINT('Origin',(70.1242640687119,50.3,10.4895355526966));
#17715=CARTESIAN_POINT('Origin',(111.7,69.7,10.4895355526966));
#17716=CARTESIAN_POINT('',(112.,69.7,10.4895355526966));
#17717=CARTESIAN_POINT('',(111.7,69.7,10.7895355526966));
#17718=CARTESIAN_POINT('Origin',(111.7,69.7,10.4895355526966));
#17719=CARTESIAN_POINT('',(111.7,70.,10.4895355526966));
#17720=CARTESIAN_POINT('Origin',(111.7,69.7,10.4895355526966));
#17721=CARTESIAN_POINT('Origin',(111.7,69.7,10.4895355526966));
#17722=CARTESIAN_POINT('Origin',(111.7,69.7,2.69738388817414));
#17723=CARTESIAN_POINT('',(112.,69.7,2.69738388817414));
#17724=CARTESIAN_POINT('',(111.7,70.,2.69738388817414));
#17725=CARTESIAN_POINT('Origin',(70.1242640687119,69.7,10.4895355526966));
#17726=CARTESIAN_POINT('',(70.1242640687119,69.7,10.7895355526966));
#17727=CARTESIAN_POINT('',(69.9121320343559,69.7,10.7016675870525));
#17728=CARTESIAN_POINT('Origin',(70.1242640687119,69.7,10.4895355526966));
#17729=CARTESIAN_POINT('',(70.1242640687119,70.,10.4895355526966));
#17730=CARTESIAN_POINT('Origin',(70.1242640687119,69.7,10.4895355526966));
#17731=CARTESIAN_POINT('Origin',(70.1242640687119,69.7,10.4895355526966));
#17732=CARTESIAN_POINT('Origin',(99.5,69.7,10.4895355526966));
#17733=CARTESIAN_POINT('',(99.5,70.,10.4895355526966));
#17734=CARTESIAN_POINT('',(99.5,69.7,10.7895355526966));
#17735=CARTESIAN_POINT('Origin',(73.1134400902689,69.7,13.4787115742535));
#17736=CARTESIAN_POINT('',(73.1134400902689,70.,13.4787115742535));
#17737=CARTESIAN_POINT('',(72.9013080559129,69.7,13.6908436086095));
#17738=CARTESIAN_POINT('Origin',(70.1242640687119,70.,10.4895355526966));
#17739=CARTESIAN_POINT('',(70.1242640687119,70.,10.7895355526966));
#17740=CARTESIAN_POINT('',(69.9121320343559,70.,10.7016675870525));
#17741=CARTESIAN_POINT('Origin',(111.7,70.,10.4895355526966));
#17742=CARTESIAN_POINT('',(112.,70.,10.4895355526966));
#17743=CARTESIAN_POINT('',(111.7,70.,10.7895355526966));
#17744=CARTESIAN_POINT('Origin',(73.1134400902689,50.3,13.4787115742535));
#17745=CARTESIAN_POINT('',(73.1134400902689,50.,13.4787115742535));
#17746=CARTESIAN_POINT('',(72.9013080559129,50.3,13.6908436086095));
#17747=CARTESIAN_POINT('Origin',(99.5,50.3,10.4895355526966));
#17748=CARTESIAN_POINT('',(99.5,50.,10.4895355526966));
#17749=CARTESIAN_POINT('',(99.5,50.3,10.7895355526966));
#17750=CARTESIAN_POINT('Origin',(74.5,69.7,3.08953555269655));
#17751=CARTESIAN_POINT('',(74.5,70.,3.08953555269655));
#17752=CARTESIAN_POINT('Origin',(62.7242640687119,70.,3.08953555269655));
#17753=CARTESIAN_POINT('',(62.512132034356,70.,3.30166758705252));
#17754=CARTESIAN_POINT('Origin',(111.7,50.3,2.69738388817414));
#17755=CARTESIAN_POINT('',(111.7,50.,2.69738388817414));
#17756=CARTESIAN_POINT('',(112.,50.3,2.69738388817414));
#17757=CARTESIAN_POINT('Origin',(111.7,70.,0.3));
#17758=CARTESIAN_POINT('',(111.7,70.,0.));
#17759=CARTESIAN_POINT('',(112.,70.,0.3));
#17760=CARTESIAN_POINT('Origin',(74.5,50.3,3.08953555269655));
#17761=CARTESIAN_POINT('',(74.5,50.,3.08953555269655));
#17762=CARTESIAN_POINT('Origin',(109.7,70.,2.48953555269655));
#17763=CARTESIAN_POINT('',(110.,70.,2.48953555269655));
#17764=CARTESIAN_POINT('Origin',(98.5,50.3,0.3));
#17765=CARTESIAN_POINT('',(110.,50.3,0.));
#17766=CARTESIAN_POINT('',(98.5,50.3,0.));
#17767=CARTESIAN_POINT('',(110.3,50.,0.3));
#17768=CARTESIAN_POINT('',(98.5,50.,0.3));
#17769=CARTESIAN_POINT('Origin',(110.3,50.3,0.3));
#17770=CARTESIAN_POINT('Origin',(110.3,50.3,4.09215166452241));
#17771=CARTESIAN_POINT('',(110.3,50.,4.09215166452241));
#17772=CARTESIAN_POINT('',(110.,50.3,4.09215166452241));
#17773=CARTESIAN_POINT('Origin',(110.,70.,2.78953555269655));
#17774=CARTESIAN_POINT('',(110.,70.,0.));
#17775=CARTESIAN_POINT('Origin',(87.,70.,5.39476777634828));
#17776=CARTESIAN_POINT('Origin',(112.,70.,0.));
#17777=CARTESIAN_POINT('Origin',(112.,70.,10.7895355526966));
#17778=CARTESIAN_POINT('',(104.475451921837,64.8,10.7895355526966));
#17779=CARTESIAN_POINT('',(77.8080528673835,64.8,10.7895355526966));
#17780=CARTESIAN_POINT('',(94.9040264336917,64.8,10.7895355526966));
#17781=CARTESIAN_POINT('',(104.475451921837,55.2,10.7895355526966));
#17782=CARTESIAN_POINT('Origin',(104.475451921837,60.,10.7895355526966));
#17783=CARTESIAN_POINT('',(77.8080528673835,55.2,10.7895355526966));
#17784=CARTESIAN_POINT('',(108.237725960918,55.2,10.7895355526966));
#17785=CARTESIAN_POINT('Origin',(77.8080528673835,60.,10.7895355526966));
#17786=CARTESIAN_POINT('Origin',(70.,70.,10.7895355526965));
#17787=CARTESIAN_POINT('Origin',(87.,50.,5.39476777634828));
#17788=CARTESIAN_POINT('Origin',(94.9040264336917,64.8,10.4895355526966));
#17789=CARTESIAN_POINT('Origin',(77.8080528673835,64.8,10.4895355526966));
#17790=CARTESIAN_POINT('Origin',(104.475451921837,64.8,10.4895355526966));
#17791=CARTESIAN_POINT('Origin',(104.475451921837,60.,10.4895355526966));
#17792=CARTESIAN_POINT('',(104.475451921837,55.5,10.4895355526966));
#17793=CARTESIAN_POINT('Origin',(104.475451921837,55.2,10.4895355526966));
#17794=CARTESIAN_POINT('Origin',(104.475451921837,60.,10.4895355526966));
#17795=CARTESIAN_POINT('Origin',(108.237725960918,55.2,10.4895355526966));
#17796=CARTESIAN_POINT('Origin',(77.8080528673835,55.2,10.4895355526966));
#17797=CARTESIAN_POINT('',(108.237725960918,55.5,10.4895355526966));
#17798=CARTESIAN_POINT('Origin',(77.8080528673835,60.,10.4895355526966));
#17799=CARTESIAN_POINT('Origin',(104.475451921837,60.,10.7895355526966));
#17800=CARTESIAN_POINT('',(104.475451921837,55.5,10.7895355526966));
#17801=CARTESIAN_POINT('Origin',(104.475451921837,55.5,10.7895355526966));
#17802=CARTESIAN_POINT('Origin',(110.,70.,0.));
#17803=CARTESIAN_POINT('',(0.,0.,0.));
#17804=CARTESIAN_POINT('',(0.,0.,0.));
#17805=CARTESIAN_POINT('',(0.,0.,0.));
#17806=CARTESIAN_POINT('',(0.,0.,0.));
#17807=CARTESIAN_POINT('',(0.,0.,0.));
#17808=CARTESIAN_POINT('',(0.,0.,0.));
#17809=CARTESIAN_POINT('',(0.,0.,0.));
#17810=CARTESIAN_POINT('',(0.,0.,0.));
#17811=CARTESIAN_POINT('',(0.,0.,0.));
#17812=CARTESIAN_POINT('',(0.,0.,0.));
#17813=UNCERTAINTY_MEASURE_WITH_UNIT(LENGTH_MEASURE(0.01),#17837,
'DISTANCE_ACCURACY_VALUE',
'Maximum model space distance between geometric entities at asserted c
onnectivities');
#17814=UNCERTAINTY_MEASURE_WITH_UNIT(LENGTH_MEASURE(0.01),#17837,
'DISTANCE_ACCURACY_VALUE',
'Maximum model space distance between geometric entities at asserted c
onnectivities');
#17815=UNCERTAINTY_MEASURE_WITH_UNIT(LENGTH_MEASURE(0.01),#17837,
'DISTANCE_ACCURACY_VALUE',
'Maximum model space distance between geometric entities at asserted c
onnectivities');
#17816=UNCERTAINTY_MEASURE_WITH_UNIT(LENGTH_MEASURE(0.01),#17837,
'DISTANCE_ACCURACY_VALUE',
'Maximum model space distance between geometric entities at asserted c
onnectivities');
#17817=UNCERTAINTY_MEASURE_WITH_UNIT(LENGTH_MEASURE(0.01),#17837,
'DISTANCE_ACCURACY_VALUE',
'Maximum model space distance between geometric entities at asserted c
onnectivities');
#17818=UNCERTAINTY_MEASURE_WITH_UNIT(LENGTH_MEASURE(0.01),#17837,
'DISTANCE_ACCURACY_VALUE',
'Maximum model space distance between geometric entities at asserted c
onnectivities');
#17819=UNCERTAINTY_MEASURE_WITH_UNIT(LENGTH_MEASURE(0.01),#17837,
'DISTANCE_ACCURACY_VALUE',
'Maximum model space distance between geometric entities at asserted c
onnectivities');
#17820=UNCERTAINTY_MEASURE_WITH_UNIT(LENGTH_MEASURE(0.01),#17837,
'DISTANCE_ACCURACY_VALUE',
'Maximum model space distance between geometric entities at asserted c
onnectivities');
#17821=UNCERTAINTY_MEASURE_WITH_UNIT(LENGTH_MEASURE(0.01),#17837,
'DISTANCE_ACCURACY_VALUE',
'Maximum model space distance between geometric entities at asserted c
onnectivities');
#17822=UNCERTAINTY_MEASURE_WITH_UNIT(LENGTH_MEASURE(0.01),#17837,
'DISTANCE_ACCURACY_VALUE',
'Maximum model space distance between geometric entities at asserted c
onnectivities');
#17823=UNCERTAINTY_MEASURE_WITH_UNIT(LENGTH_MEASURE(0.01),#17837,
'DISTANCE_ACCURACY_VALUE',
'Maximum model space distance between geometric entities at asserted c
onnectivities');
#17824=UNCERTAINTY_MEASURE_WITH_UNIT(LENGTH_MEASURE(0.01),#17837,
'DISTANCE_ACCURACY_VALUE',
'Maximum model space distance between geometric entities at asserted c
onnectivities');
#17825=(
GEOMETRIC_REPRESENTATION_CONTEXT(3)
GLOBAL_UNCERTAINTY_ASSIGNED_CONTEXT((#17813))
GLOBAL_UNIT_ASSIGNED_CONTEXT((#17837,#17839,#17840))
REPRESENTATION_CONTEXT('','3D')
);
#17826=(
GEOMETRIC_REPRESENTATION_CONTEXT(3)
GLOBAL_UNCERTAINTY_ASSIGNED_CONTEXT((#17814))
GLOBAL_UNIT_ASSIGNED_CONTEXT((#17837,#17839,#17840))
REPRESENTATION_CONTEXT('','3D')
);
#17827=(
GEOMETRIC_REPRESENTATION_CONTEXT(3)
GLOBAL_UNCERTAINTY_ASSIGNED_CONTEXT((#17815))
GLOBAL_UNIT_ASSIGNED_CONTEXT((#17837,#17839,#17840))
REPRESENTATION_CONTEXT('','3D')
);
#17828=(
GEOMETRIC_REPRESENTATION_CONTEXT(3)
GLOBAL_UNCERTAINTY_ASSIGNED_CONTEXT((#17816))
GLOBAL_UNIT_ASSIGNED_CONTEXT((#17837,#17839,#17840))
REPRESENTATION_CONTEXT('','3D')
);
#17829=(
GEOMETRIC_REPRESENTATION_CONTEXT(3)
GLOBAL_UNCERTAINTY_ASSIGNED_CONTEXT((#17817))
GLOBAL_UNIT_ASSIGNED_CONTEXT((#17837,#17839,#17840))
REPRESENTATION_CONTEXT('','3D')
);
#17830=(
GEOMETRIC_REPRESENTATION_CONTEXT(3)
GLOBAL_UNCERTAINTY_ASSIGNED_CONTEXT((#17818))
GLOBAL_UNIT_ASSIGNED_CONTEXT((#17837,#17839,#17840))
REPRESENTATION_CONTEXT('','3D')
);
#17831=(
GEOMETRIC_REPRESENTATION_CONTEXT(3)
GLOBAL_UNCERTAINTY_ASSIGNED_CONTEXT((#17819))
GLOBAL_UNIT_ASSIGNED_CONTEXT((#17837,#17839,#17840))
REPRESENTATION_CONTEXT('','3D')
);
#17832=(
GEOMETRIC_REPRESENTATION_CONTEXT(3)
GLOBAL_UNCERTAINTY_ASSIGNED_CONTEXT((#17820))
GLOBAL_UNIT_ASSIGNED_CONTEXT((#17837,#17839,#17840))
REPRESENTATION_CONTEXT('','3D')
);
#17833=(
GEOMETRIC_REPRESENTATION_CONTEXT(3)
GLOBAL_UNCERTAINTY_ASSIGNED_CONTEXT((#17821))
GLOBAL_UNIT_ASSIGNED_CONTEXT((#17837,#17839,#17840))
REPRESENTATION_CONTEXT('','3D')
);
#17834=(
GEOMETRIC_REPRESENTATION_CONTEXT(3)
GLOBAL_UNCERTAINTY_ASSIGNED_CONTEXT((#17822))
GLOBAL_UNIT_ASSIGNED_CONTEXT((#17837,#17839,#17840))
REPRESENTATION_CONTEXT('','3D')
);
#17835=(
GEOMETRIC_REPRESENTATION_CONTEXT(3)
GLOBAL_UNCERTAINTY_ASSIGNED_CONTEXT((#17823))
GLOBAL_UNIT_ASSIGNED_CONTEXT((#17837,#17839,#17840))
REPRESENTATION_CONTEXT('','3D')
);
#17836=(
GEOMETRIC_REPRESENTATION_CONTEXT(3)
GLOBAL_UNCERTAINTY_ASSIGNED_CONTEXT((#17824))
GLOBAL_UNIT_ASSIGNED_CONTEXT((#17837,#17839,#17840))
REPRESENTATION_CONTEXT('','3D')
);
#17837=(
LENGTH_UNIT()
NAMED_UNIT(*)
SI_UNIT(.MILLI.,.METRE.)
);
#17838=(
LENGTH_UNIT()
NAMED_UNIT(*)
SI_UNIT($,.METRE.)
);
#17839=(
NAMED_UNIT(*)
PLANE_ANGLE_UNIT()
SI_UNIT($,.RADIAN.)
);
#17840=(
NAMED_UNIT(*)
SI_UNIT($,.STERADIAN.)
SOLID_ANGLE_UNIT()
);
#17841=SHAPE_DEFINITION_REPRESENTATION(#17852,#17873);
#17842=SHAPE_DEFINITION_REPRESENTATION(#17853,#17874);
#17843=SHAPE_DEFINITION_REPRESENTATION(#17854,#17875);
#17844=SHAPE_DEFINITION_REPRESENTATION(#17855,#17876);
#17845=SHAPE_DEFINITION_REPRESENTATION(#17856,#17877);
#17846=SHAPE_DEFINITION_REPRESENTATION(#17857,#17878);
#17847=SHAPE_DEFINITION_REPRESENTATION(#17858,#17879);
#17848=SHAPE_DEFINITION_REPRESENTATION(#17859,#17880);
#17849=SHAPE_DEFINITION_REPRESENTATION(#17860,#17881);
#17850=SHAPE_DEFINITION_REPRESENTATION(#17861,#17882);
#17851=SHAPE_DEFINITION_REPRESENTATION(#17862,#17883);
#17852=PRODUCT_DEFINITION_SHAPE('',$,#17885);
#17853=PRODUCT_DEFINITION_SHAPE('',$,#17886);
#17854=PRODUCT_DEFINITION_SHAPE('',$,#17887);
#17855=PRODUCT_DEFINITION_SHAPE('',$,#17888);
#17856=PRODUCT_DEFINITION_SHAPE('',$,#17889);
#17857=PRODUCT_DEFINITION_SHAPE('',$,#17890);
#17858=PRODUCT_DEFINITION_SHAPE('',$,#17891);
#17859=PRODUCT_DEFINITION_SHAPE('',$,#17892);
#17860=PRODUCT_DEFINITION_SHAPE('',$,#17893);
#17861=PRODUCT_DEFINITION_SHAPE('',$,#17894);
#17862=PRODUCT_DEFINITION_SHAPE('',$,#17895);
#17863=PRODUCT_DEFINITION_SHAPE($,$,#41);
#17864=PRODUCT_DEFINITION_SHAPE($,$,#42);
#17865=PRODUCT_DEFINITION_SHAPE($,$,#43);
#17866=PRODUCT_DEFINITION_SHAPE($,$,#44);
#17867=PRODUCT_DEFINITION_SHAPE($,$,#45);
#17868=PRODUCT_DEFINITION_SHAPE($,$,#46);
#17869=PRODUCT_DEFINITION_SHAPE($,$,#47);
#17870=PRODUCT_DEFINITION_SHAPE($,$,#48);
#17871=PRODUCT_DEFINITION_SHAPE($,$,#49);
#17872=PRODUCT_DEFINITION_SHAPE($,$,#50);
#17873=SHAPE_REPRESENTATION('',(#9749,#11022,#11023,#11024,#11025,#11026,
#11027,#11028,#11029,#11030,#11031),#17825);
#17874=SHAPE_REPRESENTATION('',(#9750),#17826);
#17875=SHAPE_REPRESENTATION('',(#9764),#17827);
#17876=SHAPE_REPRESENTATION('',(#9932),#17828);
#17877=SHAPE_REPRESENTATION('',(#10101),#17829);
#17878=SHAPE_REPRESENTATION('',(#10301),#17830);
#17879=SHAPE_REPRESENTATION('',(#10399),#17831);
#17880=SHAPE_REPRESENTATION('',(#10714),#17832);
#17881=SHAPE_REPRESENTATION('',(#10812),#17833);
#17882=SHAPE_REPRESENTATION('',(#10826),#17834);
#17883=SHAPE_REPRESENTATION('',(#10924),#17835);
#17884=PRODUCT_DEFINITION_CONTEXT('part definition',#17919,'design');
#17885=PRODUCT_DEFINITION('MAS-274','MAS-274',#17896,#17884);
#17886=PRODUCT_DEFINITION('Cap_Screw_01','Cap_Screw_01',#17897,#17884);
#17887=PRODUCT_DEFINITION('Bottom_Plate','Bottom_Plate',#17898,#17884);
#17888=PRODUCT_DEFINITION('Moving_Carriage_02','Moving_Carriage_02',#17899,
#17884);
#17889=PRODUCT_DEFINITION('Top_Plate','Top_Plate',#17900,#17884);
#17890=PRODUCT_DEFINITION('Clamp_02','Clamp_02',#17901,#17884);
#17891=PRODUCT_DEFINITION('Moving_Carriage_01','Moving_Carriage_01',#17902,
#17884);
#17892=PRODUCT_DEFINITION('Clamp_01','Clamp_01',#17903,#17884);
#17893=PRODUCT_DEFINITION('Cap_Screw_02','Cap_Screw_02',#17904,#17884);
#17894=PRODUCT_DEFINITION('Clamp_03','Clamp_03',#17905,#17884);
#17895=PRODUCT_DEFINITION('Clamp_04','Clamp_04',#17906,#17884);
#17896=PRODUCT_DEFINITION_FORMATION('',$,#17921);
#17897=PRODUCT_DEFINITION_FORMATION('',$,#17922);
#17898=PRODUCT_DEFINITION_FORMATION('',$,#17923);
#17899=PRODUCT_DEFINITION_FORMATION('',$,#17924);
#17900=PRODUCT_DEFINITION_FORMATION('',$,#17925);
#17901=PRODUCT_DEFINITION_FORMATION('',$,#17926);
#17902=PRODUCT_DEFINITION_FORMATION('',$,#17927);
#17903=PRODUCT_DEFINITION_FORMATION('',$,#17928);
#17904=PRODUCT_DEFINITION_FORMATION('',$,#17929);
#17905=PRODUCT_DEFINITION_FORMATION('',$,#17930);
#17906=PRODUCT_DEFINITION_FORMATION('',$,#17931);
#17907=PRODUCT_RELATED_PRODUCT_CATEGORY('MAS-274','MAS-274',(#17921));
#17908=PRODUCT_RELATED_PRODUCT_CATEGORY('Cap_Screw_01','Cap_Screw_01',(#17922));
#17909=PRODUCT_RELATED_PRODUCT_CATEGORY('Bottom_Plate','Bottom_Plate',(#17923));
#17910=PRODUCT_RELATED_PRODUCT_CATEGORY('Moving_Carriage_02',
'Moving_Carriage_02',(#17924));
#17911=PRODUCT_RELATED_PRODUCT_CATEGORY('Top_Plate','Top_Plate',(#17925));
#17912=PRODUCT_RELATED_PRODUCT_CATEGORY('Clamp_02','Clamp_02',(#17926));
#17913=PRODUCT_RELATED_PRODUCT_CATEGORY('Moving_Carriage_01',
'Moving_Carriage_01',(#17927));
#17914=PRODUCT_RELATED_PRODUCT_CATEGORY('Clamp_01','Clamp_01',(#17928));
#17915=PRODUCT_RELATED_PRODUCT_CATEGORY('Cap_Screw_02','Cap_Screw_02',(#17929));
#17916=PRODUCT_RELATED_PRODUCT_CATEGORY('Clamp_03','Clamp_03',(#17930));
#17917=PRODUCT_RELATED_PRODUCT_CATEGORY('Clamp_04','Clamp_04',(#17931));
#17918=APPLICATION_PROTOCOL_DEFINITION('international standard',
'automotive_design',2009,#17919);
#17919=APPLICATION_CONTEXT(
'Core Data for Automotive Mechanical Design Process');
#17920=PRODUCT_CONTEXT('part definition',#17919,'mechanical');
#17921=PRODUCT('MAS-274','MAS-274',$,(#17920));
#17922=PRODUCT('Cap_Screw_01','Cap_Screw_01',$,(#17920));
#17923=PRODUCT('Bottom_Plate','Bottom_Plate',$,(#17920));
#17924=PRODUCT('Moving_Carriage_02','Moving_Carriage_02',$,(#17920));
#17925=PRODUCT('Top_Plate','Top_Plate',$,(#17920));
#17926=PRODUCT('Clamp_02','Clamp_02',$,(#17920));
#17927=PRODUCT('Moving_Carriage_01','Moving_Carriage_01',$,(#17920));
#17928=PRODUCT('Clamp_01','Clamp_01',$,(#17920));
#17929=PRODUCT('Cap_Screw_02','Cap_Screw_02',$,(#17920));
#17930=PRODUCT('Clamp_03','Clamp_03',$,(#17920));
#17931=PRODUCT('Clamp_04','Clamp_04',$,(#17920));
#17932=PRESENTATION_STYLE_ASSIGNMENT((#17934));
#17933=PRESENTATION_STYLE_ASSIGNMENT((#17935));
#17934=SURFACE_STYLE_USAGE(.BOTH.,#17936);
#17935=SURFACE_STYLE_USAGE(.BOTH.,#17937);
#17936=SURFACE_SIDE_STYLE('',(#17938));
#17937=SURFACE_SIDE_STYLE('',(#17939));
#17938=SURFACE_STYLE_FILL_AREA(#17940);
#17939=SURFACE_STYLE_FILL_AREA(#17941);
#17940=FILL_AREA_STYLE('Steel - Satin',(#17942));
#17941=FILL_AREA_STYLE('Steel - Satin',(#17943));
#17942=FILL_AREA_STYLE_COLOUR('Steel - Satin',#17944);
#17943=FILL_AREA_STYLE_COLOUR('Steel - Satin',#17945);
#17944=COLOUR_RGB('Steel - Satin',0.627450980392157,0.627450980392157,0.627450980392157);
#17945=COLOUR_RGB('Steel - Satin',0.290196078431373,0.290196078431373,0.290196078431373);
#17946=COLOUR_RGB('Dark Blue',0.08,0.2,0.34);
#17947=FILL_AREA_STYLE_COLOUR('',#17946);
#17948=FILL_AREA_STYLE('',(#17947));
#17949=SURFACE_STYLE_FILL_AREA(#17948);
#17950=SURFACE_SIDE_STYLE('',(#17949));
#17951=SURFACE_STYLE_USAGE(.BOTH.,#17950);
#17952=PRESENTATION_STYLE_ASSIGNMENT((#17951));
#17953=COLOUR_RGB('Light Blue',0.38,0.62,0.78);
#17954=FILL_AREA_STYLE_COLOUR('',#17953);
#17955=FILL_AREA_STYLE('',(#17954));
#17956=SURFACE_STYLE_FILL_AREA(#17955);
#17957=SURFACE_SIDE_STYLE('',(#17956));
#17958=SURFACE_STYLE_USAGE(.BOTH.,#17957);
#17959=PRESENTATION_STYLE_ASSIGNMENT((#17958));
#17960=COLOUR_RGB('Sky Blue',0.24,0.69,0.87);
#17961=FILL_AREA_STYLE_COLOUR('',#17960);
#17962=FILL_AREA_STYLE('',(#17961));
#17963=SURFACE_STYLE_FILL_AREA(#17962);
#17964=SURFACE_SIDE_STYLE('',(#17963));
#17965=SURFACE_STYLE_USAGE(.BOTH.,#17964);
#17966=PRESENTATION_STYLE_ASSIGNMENT((#17965));
#17967=COLOUR_RGB('Grey',0.48,0.52,0.57);
#17968=FILL_AREA_STYLE_COLOUR('',#17967);
#17969=FILL_AREA_STYLE('',(#17968));
#17970=SURFACE_STYLE_FILL_AREA(#17969);
#17971=SURFACE_SIDE_STYLE('',(#17970));
#17972=SURFACE_STYLE_USAGE(.BOTH.,#17971);
#17973=PRESENTATION_STYLE_ASSIGNMENT((#17972));
#17974=COLOUR_RGB('Black',0.12,0.14,0.17);
#17975=FILL_AREA_STYLE_COLOUR('',#17974);
#17976=FILL_AREA_STYLE('',(#17975));
#17977=SURFACE_STYLE_FILL_AREA(#17976);
#17978=SURFACE_SIDE_STYLE('',(#17977));
#17979=SURFACE_STYLE_USAGE(.BOTH.,#17978);
#17980=PRESENTATION_STYLE_ASSIGNMENT((#17979));
#17981=COLOUR_RGB('Off White',0.89,0.88,0.83);
#17982=FILL_AREA_STYLE_COLOUR('',#17981);
#17983=FILL_AREA_STYLE('',(#17982));
#17984=SURFACE_STYLE_FILL_AREA(#17983);
#17985=SURFACE_SIDE_STYLE('',(#17984));
#17986=SURFACE_STYLE_USAGE(.BOTH.,#17985);
#17987=PRESENTATION_STYLE_ASSIGNMENT((#17986));
ENDSEC;
END-ISO-10303-21;
